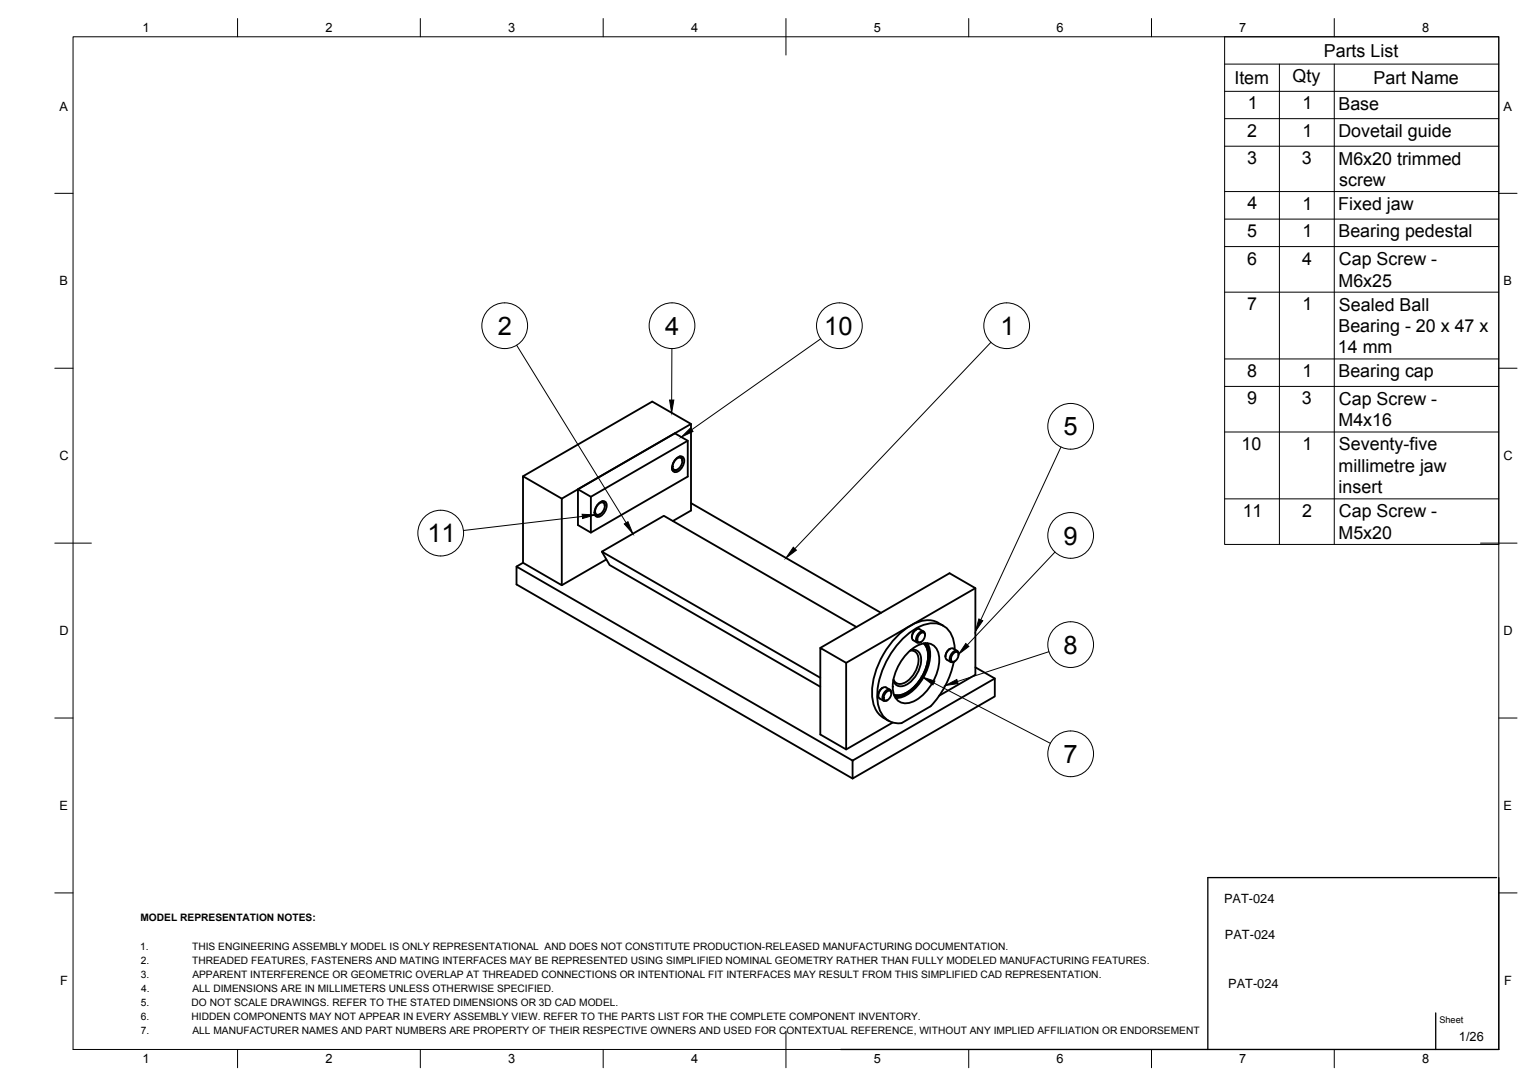
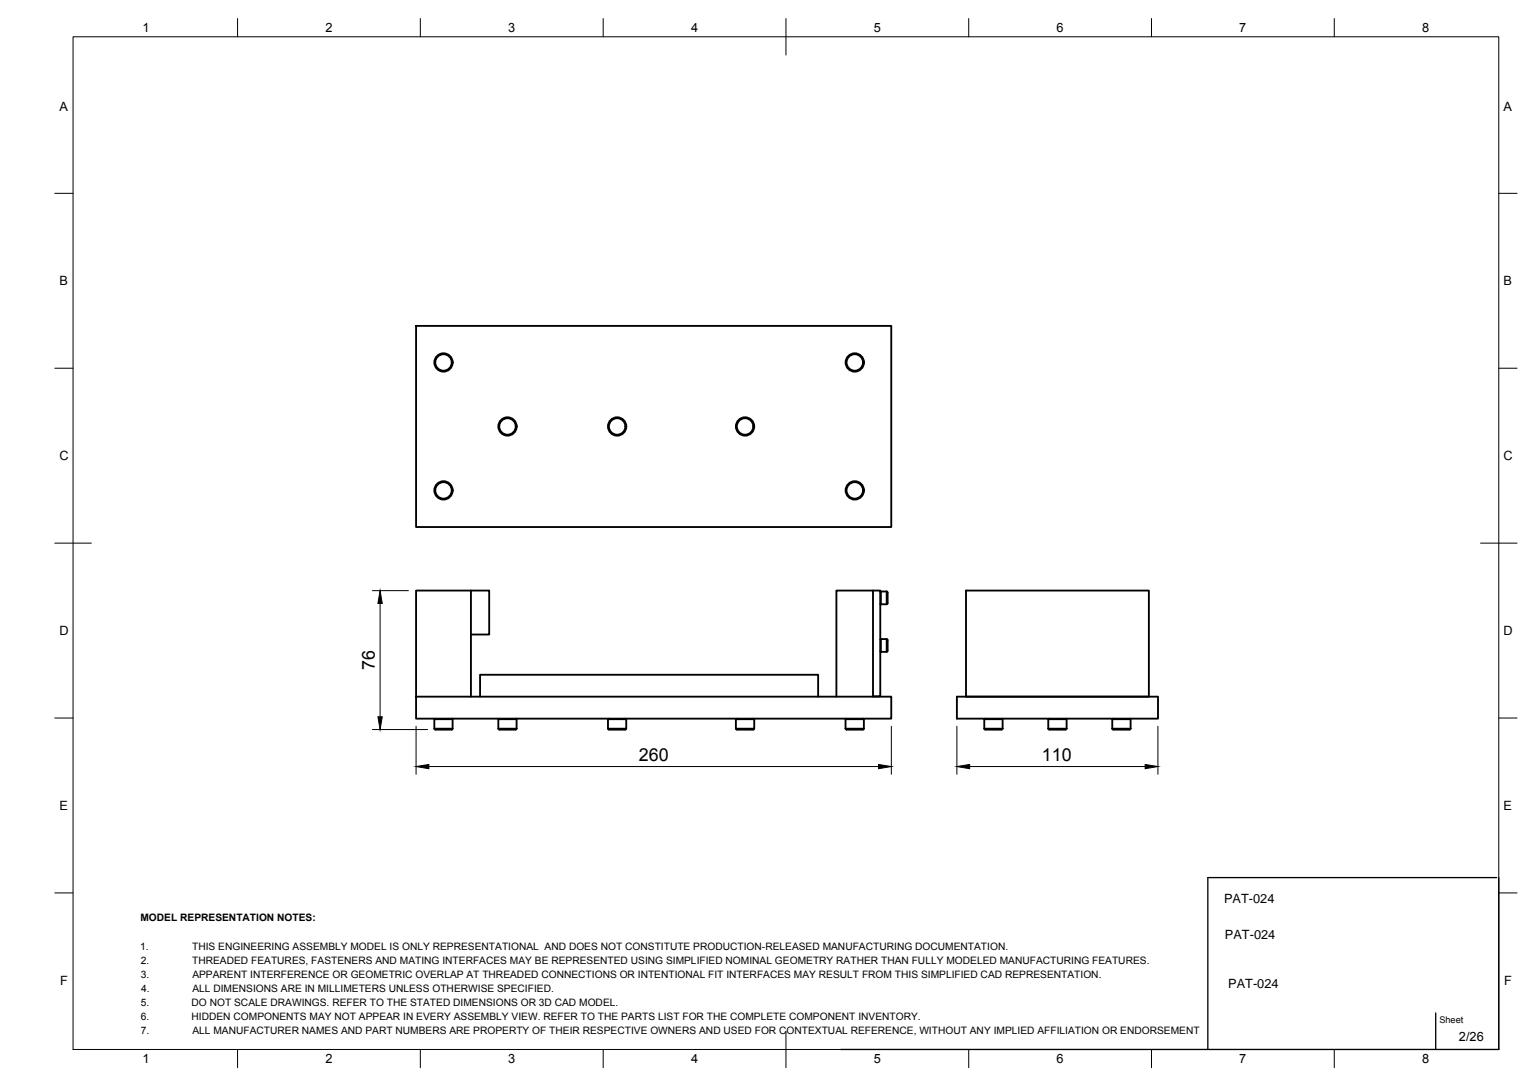
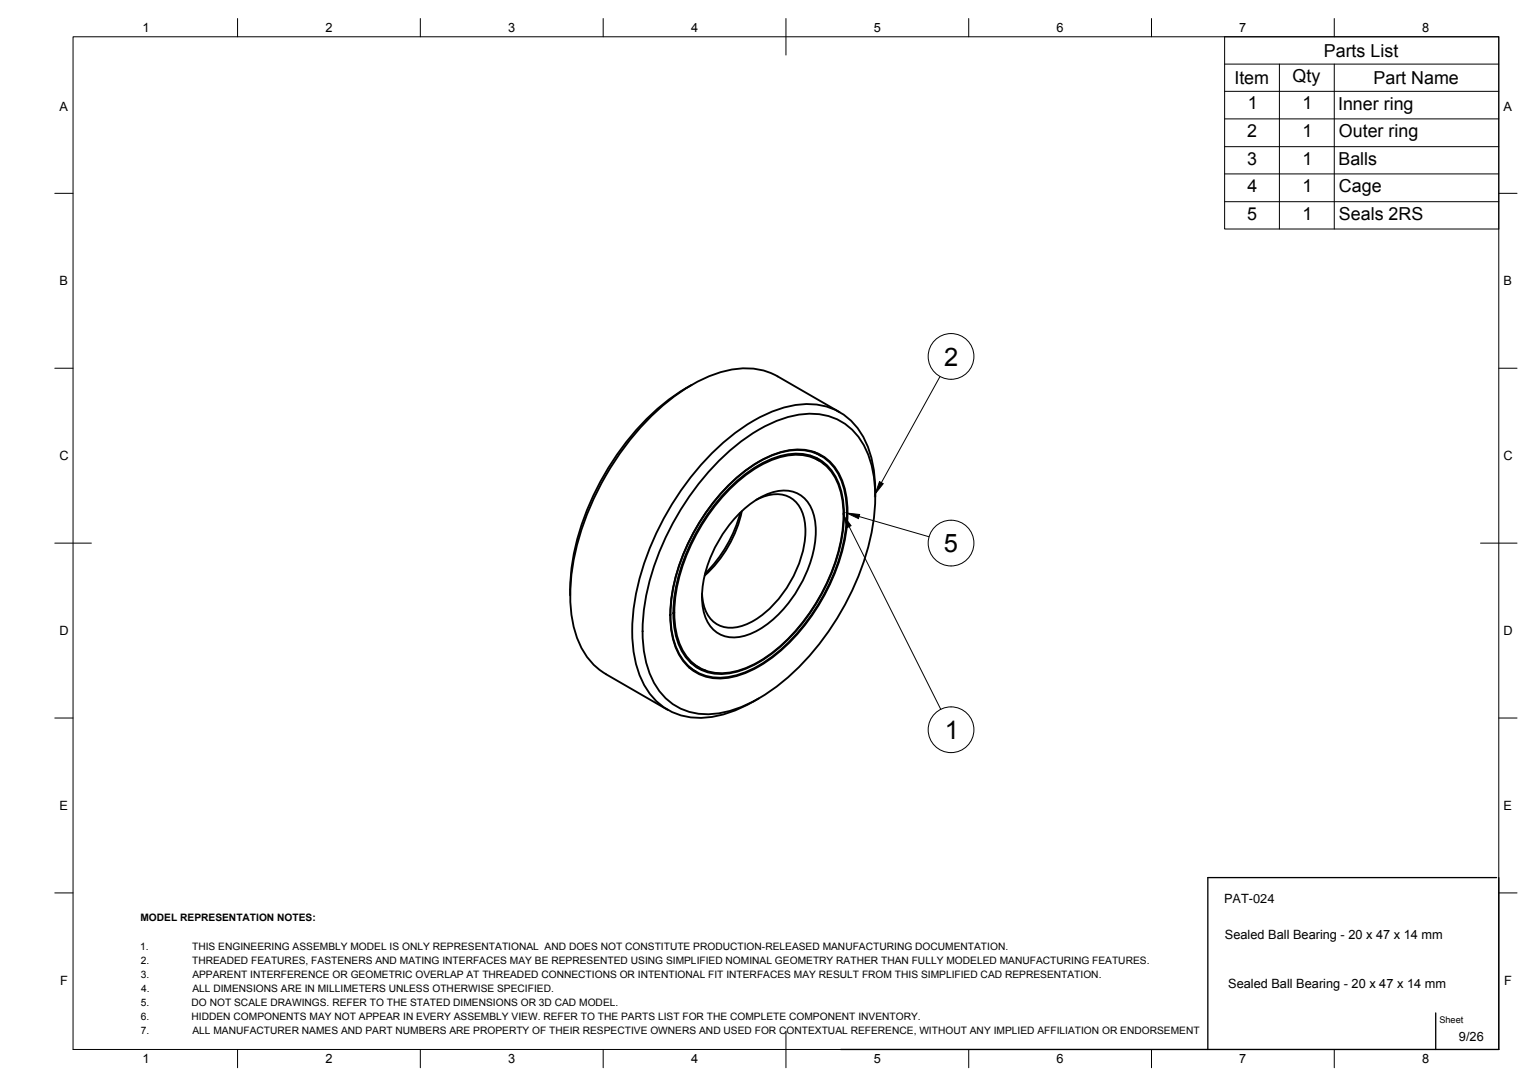
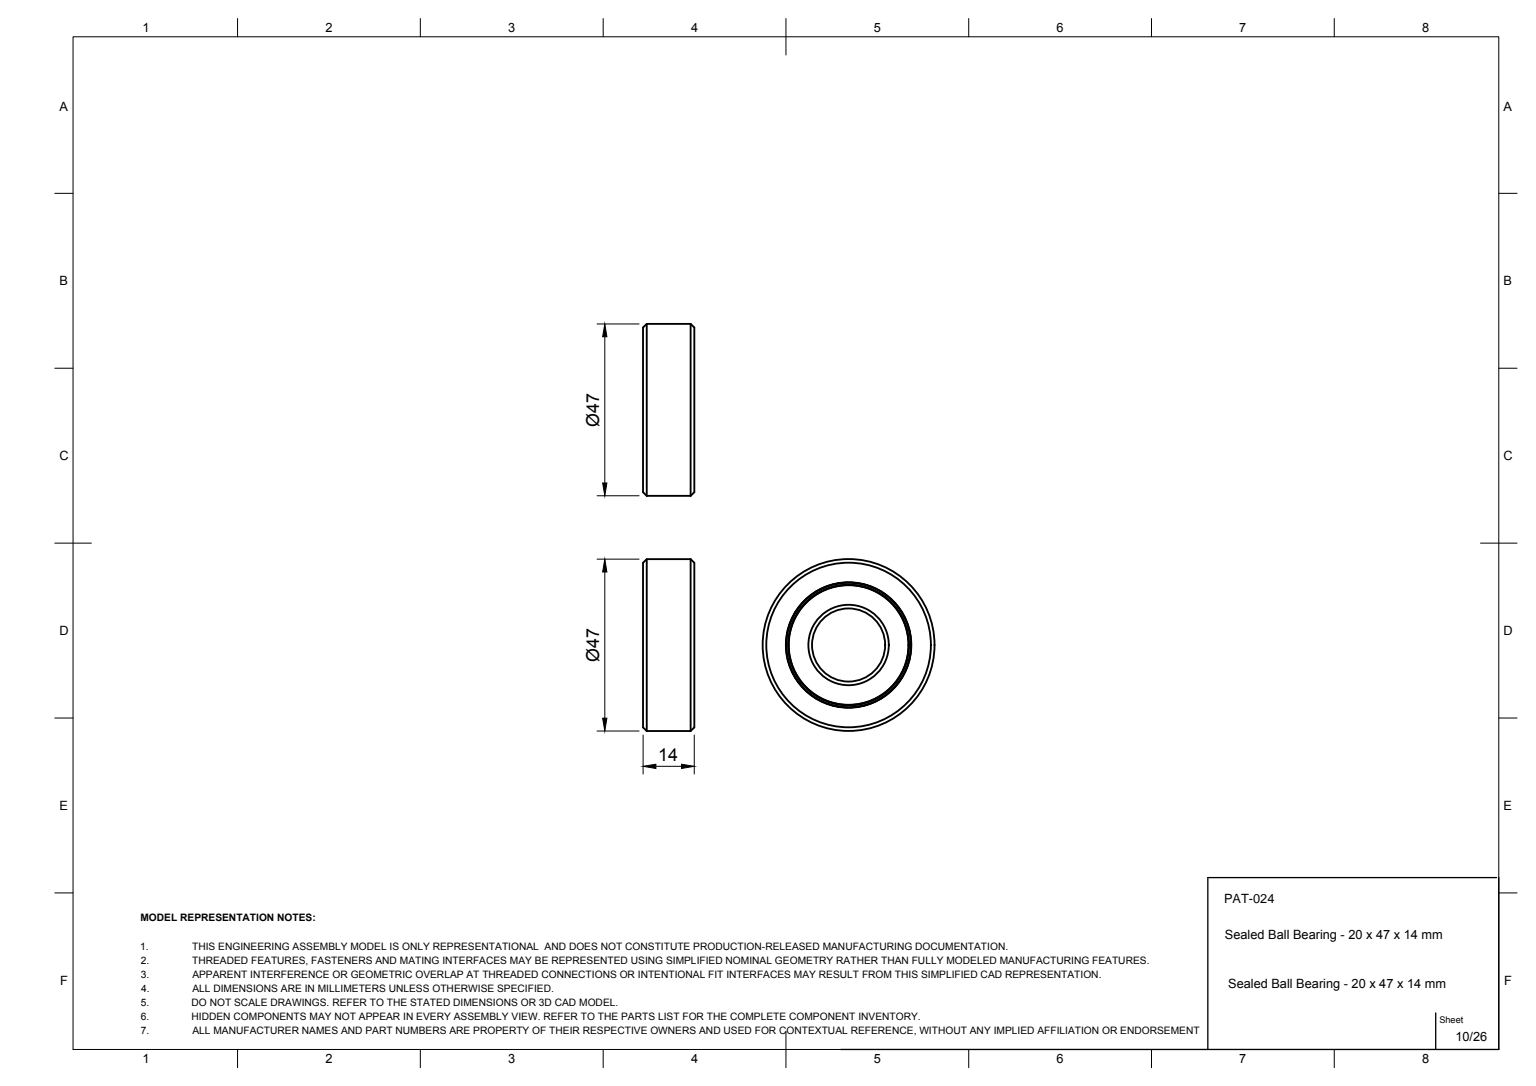
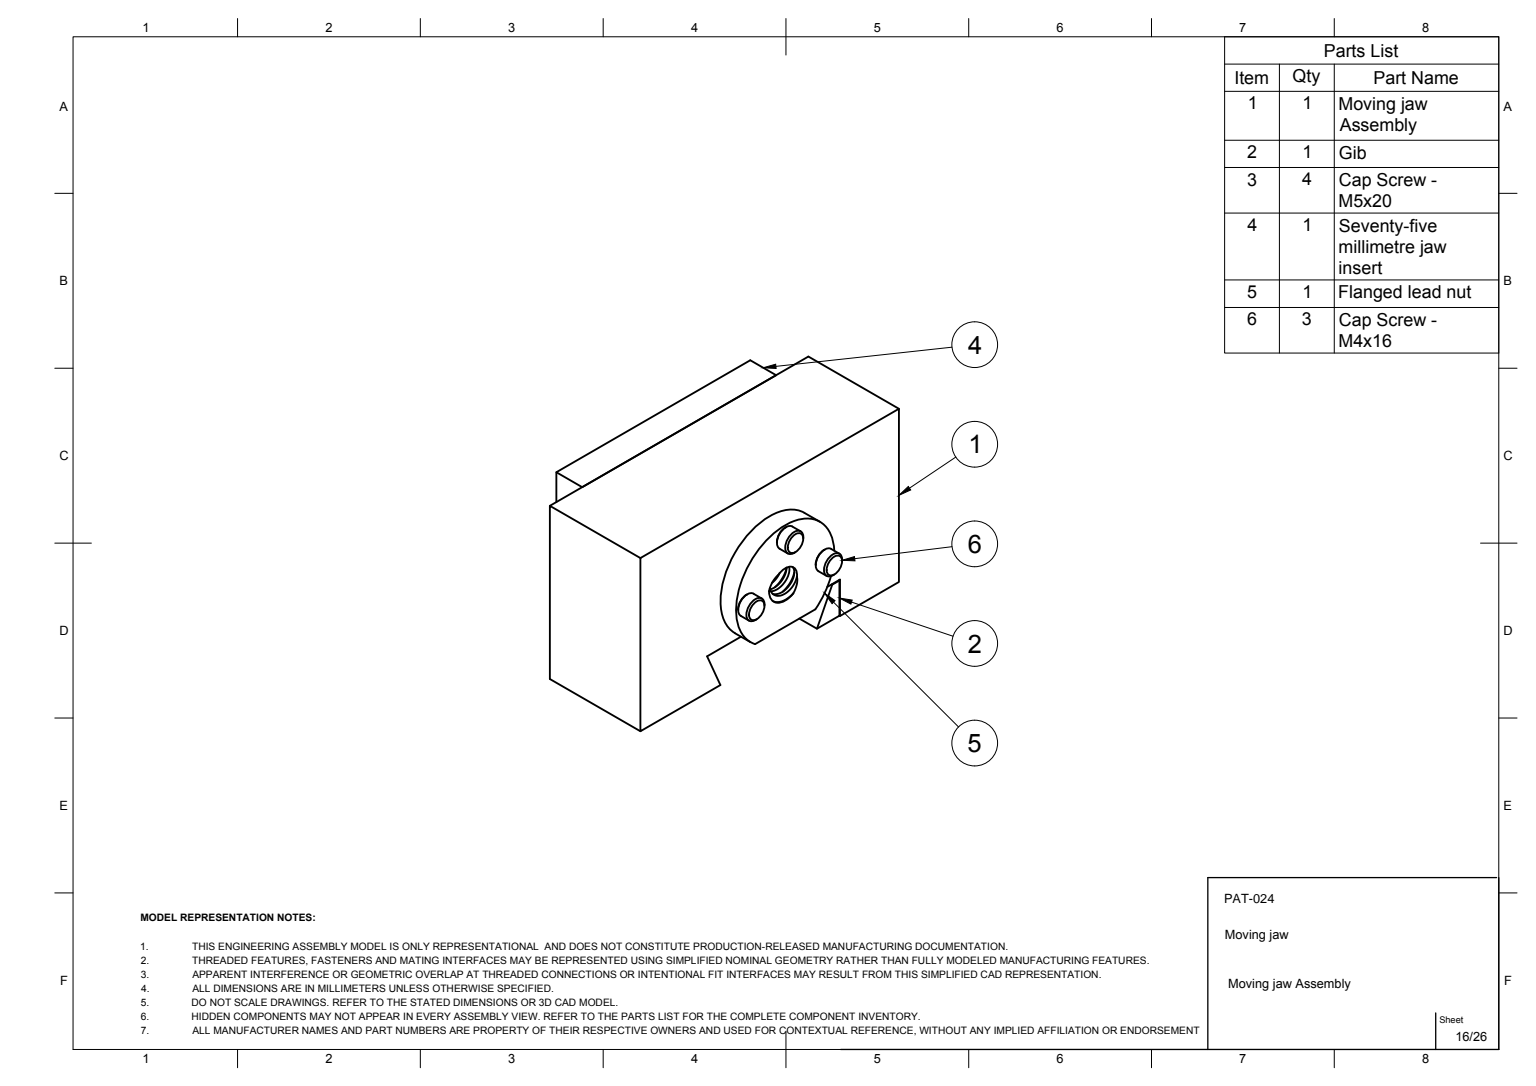
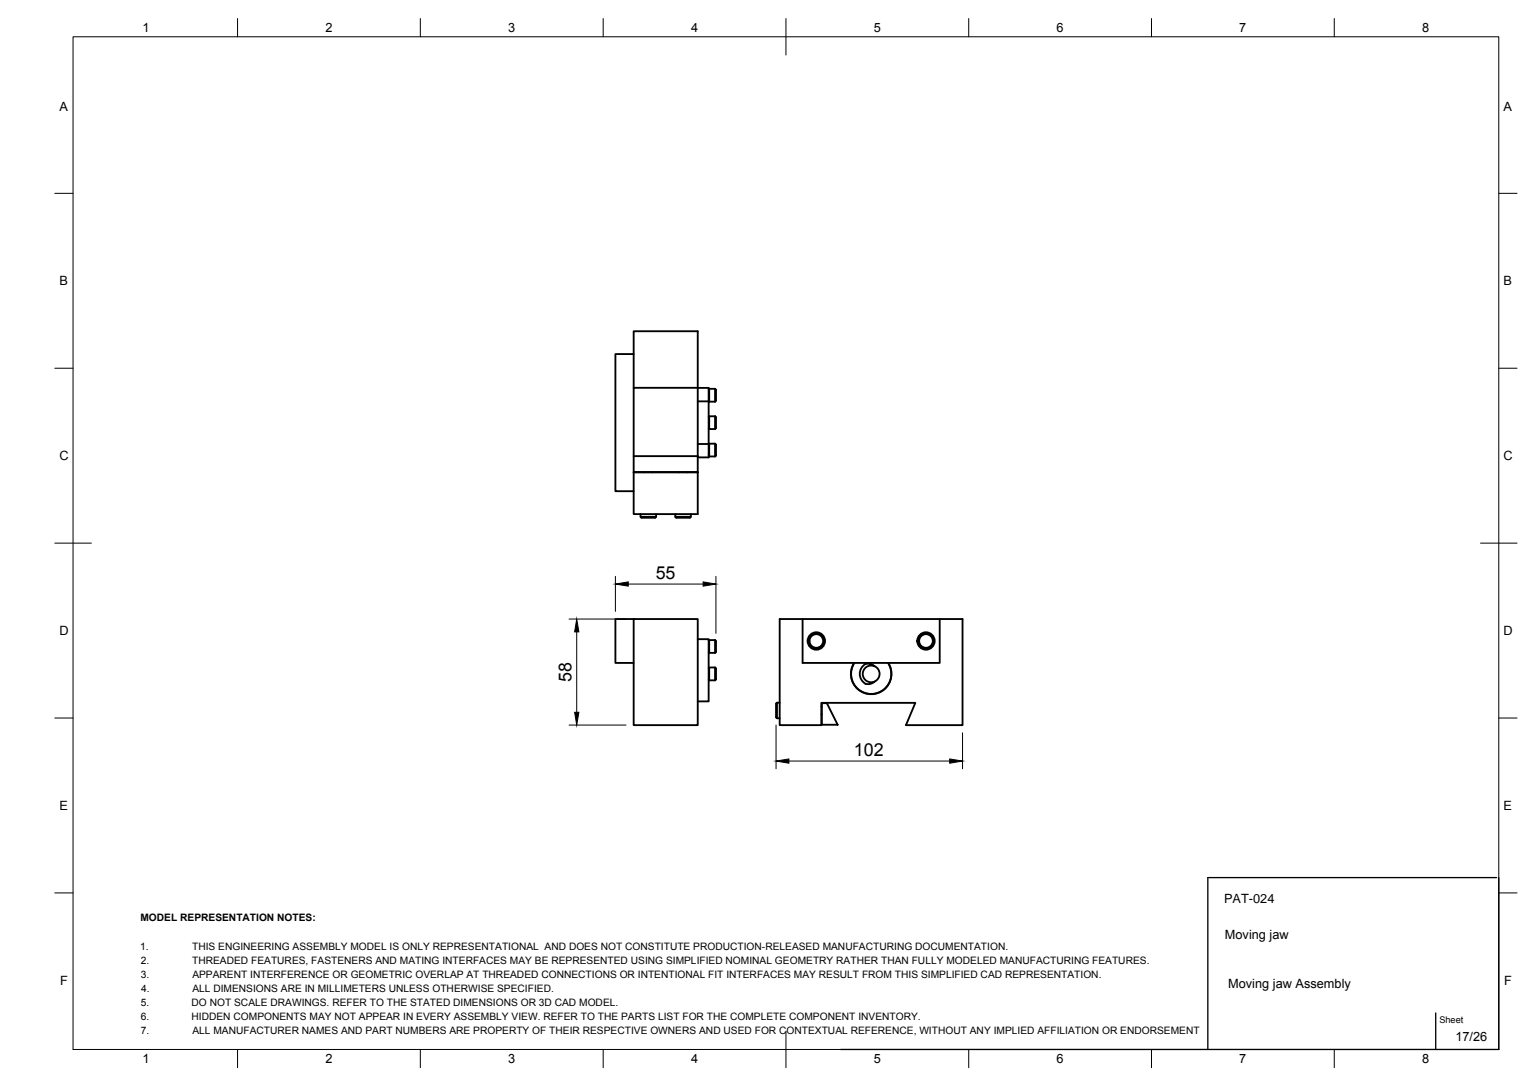
ISO-10303-21;
HEADER;
/* Generated by software containing ST-Developer
 * from STEP Tools, Inc. (www.steptools.com) 
 */

FILE_DESCRIPTION(
/* description */ ('Compact handwheel screw vise'),
/* implementation_level */ '2;1');

FILE_NAME(
/* name */ 'PAT-024',
/* time_stamp */ '2026-10-29T16:08:22-07:00',
/* author */ (''),
/* organization */ (''),
/* preprocessor_version */ 'ST-DEVELOPER v20.2',
/* originating_system */ 'Autodesk Translation Framework v15.17.0.0',
/* authorisation */ '');

FILE_SCHEMA (('AUTOMOTIVE_DESIGN { 1 0 10303 214 3 1 1 }'));
ENDSEC;

DATA;
#10=MECHANICAL_DESIGN_GEOMETRIC_PRESENTATION_REPRESENTATION('',(#644,#645,
#646,#647,#648,#649,#650,#651,#652,#653,#654,#655,#656,#657,#658,#659,#660,
#661,#662,#663,#664,#665,#666,#667,#668,#669,#670,#671,#672,#673,#674,#675,
#676,#677,#678,#679),#25074);
#11=B_SPLINE_SURFACE_WITH_KNOTS('',3,3,((#13564,#13565,#13566,#13567,#13568,
#13569,#13570,#13571,#13572,#13573,#13574,#13575,#13576,#13577,#13578,#13579,
#13580,#13581,#13582,#13583,#13584,#13585,#13586,#13587,#13588,#13589,#13590,
#13591,#13592,#13593,#13594,#13595,#13596,#13597,#13598,#13599,#13600,#13601,
#13602,#13603,#13604,#13605,#13606,#13607,#13608,#13609,#13610,#13611,#13612,
#13613,#13614,#13615,#13616,#13617,#13618,#13619,#13620,#13621,#13622,#13623,
#13624,#13625,#13626,#13627,#13628,#13629,#13630,#13631,#13632,#13633,#13634,
#13635,#13636,#13637,#13638,#13639,#13640,#13641,#13642,#13643,#13644,#13645,
#13646,#13647,#13648,#13649,#13650,#13651,#13652,#13653,#13654,#13655,#13656,
#13657,#13658,#13659,#13660,#13661,#13662,#13663,#13664,#13665,#13666,#13667,
#13668,#13669,#13670,#13671,#13672,#13673,#13674,#13675,#13676,#13677,#13678),
(#13679,#13680,#13681,#13682,#13683,#13684,#13685,#13686,#13687,#13688,
#13689,#13690,#13691,#13692,#13693,#13694,#13695,#13696,#13697,#13698,#13699,
#13700,#13701,#13702,#13703,#13704,#13705,#13706,#13707,#13708,#13709,#13710,
#13711,#13712,#13713,#13714,#13715,#13716,#13717,#13718,#13719,#13720,#13721,
#13722,#13723,#13724,#13725,#13726,#13727,#13728,#13729,#13730,#13731,#13732,
#13733,#13734,#13735,#13736,#13737,#13738,#13739,#13740,#13741,#13742,#13743,
#13744,#13745,#13746,#13747,#13748,#13749,#13750,#13751,#13752,#13753,#13754,
#13755,#13756,#13757,#13758,#13759,#13760,#13761,#13762,#13763,#13764,#13765,
#13766,#13767,#13768,#13769,#13770,#13771,#13772,#13773,#13774,#13775,#13776,
#13777,#13778,#13779,#13780,#13781,#13782,#13783,#13784,#13785,#13786,#13787,
#13788,#13789,#13790,#13791,#13792,#13793),(#13794,#13795,#13796,#13797,
#13798,#13799,#13800,#13801,#13802,#13803,#13804,#13805,#13806,#13807,#13808,
#13809,#13810,#13811,#13812,#13813,#13814,#13815,#13816,#13817,#13818,#13819,
#13820,#13821,#13822,#13823,#13824,#13825,#13826,#13827,#13828,#13829,#13830,
#13831,#13832,#13833,#13834,#13835,#13836,#13837,#13838,#13839,#13840,#13841,
#13842,#13843,#13844,#13845,#13846,#13847,#13848,#13849,#13850,#13851,#13852,
#13853,#13854,#13855,#13856,#13857,#13858,#13859,#13860,#13861,#13862,#13863,
#13864,#13865,#13866,#13867,#13868,#13869,#13870,#13871,#13872,#13873,#13874,
#13875,#13876,#13877,#13878,#13879,#13880,#13881,#13882,#13883,#13884,#13885,
#13886,#13887,#13888,#13889,#13890,#13891,#13892,#13893,#13894,#13895,#13896,
#13897,#13898,#13899,#13900,#13901,#13902,#13903,#13904,#13905,#13906,#13907,
#13908),(#13909,#13910,#13911,#13912,#13913,#13914,#13915,#13916,#13917,
#13918,#13919,#13920,#13921,#13922,#13923,#13924,#13925,#13926,#13927,#13928,
#13929,#13930,#13931,#13932,#13933,#13934,#13935,#13936,#13937,#13938,#13939,
#13940,#13941,#13942,#13943,#13944,#13945,#13946,#13947,#13948,#13949,#13950,
#13951,#13952,#13953,#13954,#13955,#13956,#13957,#13958,#13959,#13960,#13961,
#13962,#13963,#13964,#13965,#13966,#13967,#13968,#13969,#13970,#13971,#13972,
#13973,#13974,#13975,#13976,#13977,#13978,#13979,#13980,#13981,#13982,#13983,
#13984,#13985,#13986,#13987,#13988,#13989,#13990,#13991,#13992,#13993,#13994,
#13995,#13996,#13997,#13998,#13999,#14000,#14001,#14002,#14003,#14004,#14005,
#14006,#14007,#14008,#14009,#14010,#14011,#14012,#14013,#14014,#14015,#14016,
#14017,#14018,#14019,#14020,#14021,#14022,#14023)),.UNSPECIFIED.,.F.,.F.,
 .F.,(4,4),(4,1,1,1,1,1,1,1,1,1,1,1,1,1,1,1,1,1,1,1,1,1,1,1,1,1,1,1,1,1,
1,1,1,1,1,1,1,1,1,1,1,1,1,1,1,1,1,1,1,1,1,1,1,1,1,1,1,1,1,1,1,1,1,1,1,1,
1,1,1,1,1,1,1,1,1,1,1,1,1,1,1,1,1,1,1,1,1,1,1,1,1,1,1,1,1,1,1,1,1,1,1,1,
1,1,1,1,1,1,1,1,1,1,4),(0.,0.173020531651036),(12.1475814751569,12.6421543672732,
13.1367272593894,13.6313001515056,14.1258730436219,14.6204459357381,15.1150188278544,
15.6095917199706,16.1041646120869,16.5987375042031,17.0933103963194,17.5878832884356,
18.0824561805519,18.5770290726681,19.0716019647843,19.5661748569006,20.0607477490168,
20.5553206411331,21.0498935332493,21.5444664253656,22.0390393174818,22.5336122095981,
23.0281851017143,23.5227579938306,24.0173308859468,24.511903778063,25.0064766701793,
25.5010495622955,25.9956224544118,26.490195346528,26.9847682386443,27.4793411307605,
27.9739140228768,28.468486914993,28.9630598071093,29.4576326992255,29.9522055913417,
30.446778483458,30.9413513755742,31.4359242676905,31.9304971598067,32.425070051923,
32.9196429440392,33.4142158361555,33.9087887282717,34.403361620388,34.8979345125042,
35.3925074046204,35.8870802967367,36.3816531888529,36.8762260809692,37.3707989730854,
37.8653718652017,38.3599447573179,38.8545176494342,39.3490905415504,39.8436634336667,
40.3382363257829,40.8328092178991,41.3273821100154,41.8219550021316,42.3165278942479,
42.8111007863641,43.3056736784804,43.8002465705966,44.2948194627129,44.7893923548291,
45.2839652469454,45.7785381390616,46.2731110311778,46.7676839232941,47.2622568154103,
47.7568297075266,48.2514025996428,48.7459754917591,49.2405483838753,49.7351212759916,
50.2296941681078,50.7242670602241,51.2188399523403,51.7134128444565,52.2079857365728,
52.702558628689,53.1971315208053,53.6917044129215,54.1862773050378,54.680850197154,
55.1754230892703,55.6699959813865,56.1645688735028,56.659141765619,57.1537146577353,
57.6482875498515,58.1428604419677,58.637433334084,59.1320062262002,59.6265791183165,
60.1211520104327,60.615724902549,61.1102977946652,61.6048706867815,62.0994435788977,
62.5940164710139,63.0885893631302,63.5831622552464,64.0777351473627,64.5723080394789,
65.0668809315952,65.5614538237114,66.0560267158277,66.5505996079439,67.0451725000601,
67.5397453921764),.UNSPECIFIED.);
#12=B_SPLINE_SURFACE_WITH_KNOTS('',3,3,((#14123,#14124,#14125,#14126,#14127,
#14128,#14129,#14130,#14131,#14132,#14133,#14134,#14135,#14136,#14137,#14138,
#14139,#14140,#14141,#14142,#14143,#14144,#14145,#14146,#14147,#14148,#14149,
#14150,#14151,#14152,#14153,#14154,#14155,#14156,#14157,#14158,#14159,#14160,
#14161,#14162,#14163,#14164,#14165,#14166,#14167,#14168,#14169,#14170,#14171,
#14172,#14173,#14174,#14175,#14176,#14177,#14178,#14179,#14180,#14181,#14182,
#14183,#14184,#14185,#14186,#14187,#14188,#14189,#14190,#14191,#14192,#14193,
#14194,#14195,#14196,#14197,#14198,#14199,#14200,#14201,#14202,#14203,#14204,
#14205,#14206,#14207,#14208,#14209,#14210,#14211,#14212,#14213,#14214,#14215,
#14216,#14217,#14218,#14219,#14220,#14221,#14222,#14223,#14224,#14225,#14226,
#14227,#14228,#14229,#14230,#14231,#14232,#14233,#14234,#14235,#14236,#14237),
(#14238,#14239,#14240,#14241,#14242,#14243,#14244,#14245,#14246,#14247,
#14248,#14249,#14250,#14251,#14252,#14253,#14254,#14255,#14256,#14257,#14258,
#14259,#14260,#14261,#14262,#14263,#14264,#14265,#14266,#14267,#14268,#14269,
#14270,#14271,#14272,#14273,#14274,#14275,#14276,#14277,#14278,#14279,#14280,
#14281,#14282,#14283,#14284,#14285,#14286,#14287,#14288,#14289,#14290,#14291,
#14292,#14293,#14294,#14295,#14296,#14297,#14298,#14299,#14300,#14301,#14302,
#14303,#14304,#14305,#14306,#14307,#14308,#14309,#14310,#14311,#14312,#14313,
#14314,#14315,#14316,#14317,#14318,#14319,#14320,#14321,#14322,#14323,#14324,
#14325,#14326,#14327,#14328,#14329,#14330,#14331,#14332,#14333,#14334,#14335,
#14336,#14337,#14338,#14339,#14340,#14341,#14342,#14343,#14344,#14345,#14346,
#14347,#14348,#14349,#14350,#14351,#14352),(#14353,#14354,#14355,#14356,
#14357,#14358,#14359,#14360,#14361,#14362,#14363,#14364,#14365,#14366,#14367,
#14368,#14369,#14370,#14371,#14372,#14373,#14374,#14375,#14376,#14377,#14378,
#14379,#14380,#14381,#14382,#14383,#14384,#14385,#14386,#14387,#14388,#14389,
#14390,#14391,#14392,#14393,#14394,#14395,#14396,#14397,#14398,#14399,#14400,
#14401,#14402,#14403,#14404,#14405,#14406,#14407,#14408,#14409,#14410,#14411,
#14412,#14413,#14414,#14415,#14416,#14417,#14418,#14419,#14420,#14421,#14422,
#14423,#14424,#14425,#14426,#14427,#14428,#14429,#14430,#14431,#14432,#14433,
#14434,#14435,#14436,#14437,#14438,#14439,#14440,#14441,#14442,#14443,#14444,
#14445,#14446,#14447,#14448,#14449,#14450,#14451,#14452,#14453,#14454,#14455,
#14456,#14457,#14458,#14459,#14460,#14461,#14462,#14463,#14464,#14465,#14466,
#14467),(#14468,#14469,#14470,#14471,#14472,#14473,#14474,#14475,#14476,
#14477,#14478,#14479,#14480,#14481,#14482,#14483,#14484,#14485,#14486,#14487,
#14488,#14489,#14490,#14491,#14492,#14493,#14494,#14495,#14496,#14497,#14498,
#14499,#14500,#14501,#14502,#14503,#14504,#14505,#14506,#14507,#14508,#14509,
#14510,#14511,#14512,#14513,#14514,#14515,#14516,#14517,#14518,#14519,#14520,
#14521,#14522,#14523,#14524,#14525,#14526,#14527,#14528,#14529,#14530,#14531,
#14532,#14533,#14534,#14535,#14536,#14537,#14538,#14539,#14540,#14541,#14542,
#14543,#14544,#14545,#14546,#14547,#14548,#14549,#14550,#14551,#14552,#14553,
#14554,#14555,#14556,#14557,#14558,#14559,#14560,#14561,#14562,#14563,#14564,
#14565,#14566,#14567,#14568,#14569,#14570,#14571,#14572,#14573,#14574,#14575,
#14576,#14577,#14578,#14579,#14580,#14581,#14582)),.UNSPECIFIED.,.F.,.F.,
 .F.,(4,4),(4,1,1,1,1,1,1,1,1,1,1,1,1,1,1,1,1,1,1,1,1,1,1,1,1,1,1,1,1,1,
1,1,1,1,1,1,1,1,1,1,1,1,1,1,1,1,1,1,1,1,1,1,1,1,1,1,1,1,1,1,1,1,1,1,1,1,
1,1,1,1,1,1,1,1,1,1,1,1,1,1,1,1,1,1,1,1,1,1,1,1,1,1,1,1,1,1,1,1,1,1,1,1,
1,1,1,1,1,1,1,1,1,1,4),(0.,0.173020531651036),(15.1888611523549,15.6834340444711,
16.1780069365874,16.6725798287036,17.1671527208199,17.6617256129361,18.1562985050523,
18.6508713971686,19.1454442892848,19.6400171814011,20.1345900735173,20.6291629656336,
21.1237358577498,21.6183087498661,22.1128816419823,22.6074545340986,23.1020274262148,
23.596600318331,24.0911732104473,24.5857461025635,25.0803189946798,25.574891886796,
26.0694647789123,26.5640376710285,27.0586105631448,27.553183455261,28.0477563473773,
28.5423292394935,29.0369021316097,29.531475023726,30.0260479158422,30.5206208079585,
31.0151937000747,31.509766592191,32.0043394843072,32.4989123764235,32.9934852685397,
33.488058160656,33.9826310527722,34.4772039448884,34.9717768370047,35.4663497291209,
35.9609226212372,36.4554955133534,36.9500684054697,37.4446412975859,37.9392141897022,
38.4337870818184,38.9283599739347,39.4229328660509,39.9175057581671,40.4120786502834,
40.9066515423996,41.4012244345159,41.8957973266321,42.3903702187484,42.8849431108646,
43.3795160029809,43.8740888950971,44.3686617872134,44.8632346793296,45.3578075714458,
45.8523804635621,46.3469533556783,46.8415262477946,47.3360991399108,47.8306720320271,
48.3252449241433,48.8198178162596,49.3143907083758,49.8089636004921,50.3035364926083,
50.7981093847245,51.2926822768408,51.787255168957,52.2818280610733,52.7764009531895,
53.2709738453058,53.765546737422,54.2601196295383,54.7546925216545,55.2492654137708,
55.743838305887,56.2384111980032,56.7329840901195,57.2275569822357,57.722129874352,
58.2167027664682,58.7112756585845,59.2058485507007,59.700421442817,60.1949943349332,
60.6895672270495,61.1841401191657,61.6787130112819,62.1732859033982,62.6678587955144,
63.1624316876307,63.6570045797469,64.1515774718632,64.6461503639794,65.1407232560957,
65.6352961482119,66.1298690403281,66.6244419324444,67.1190148245607,67.6135877166769,
68.1081606087931,68.6027335009094,69.0973063930256,69.5918792851419,70.0864521772581,
70.5810250693744),.UNSPECIFIED.);
#13=B_SPLINE_SURFACE_WITH_KNOTS('',3,3,((#20271,#20272,#20273,#20274,#20275,
#20276,#20277,#20278,#20279,#20280,#20281,#20282,#20283,#20284,#20285,#20286,
#20287,#20288,#20289,#20290,#20291,#20292,#20293,#20294,#20295,#20296,#20297,
#20298,#20299,#20300,#20301,#20302,#20303,#20304,#20305,#20306,#20307,#20308,
#20309,#20310,#20311,#20312,#20313,#20314,#20315,#20316,#20317,#20318,#20319,
#20320,#20321,#20322,#20323,#20324,#20325,#20326,#20327,#20328,#20329,#20330,
#20331,#20332,#20333,#20334,#20335,#20336,#20337,#20338,#20339,#20340,#20341,
#20342,#20343,#20344,#20345,#20346,#20347,#20348,#20349,#20350,#20351,#20352,
#20353,#20354,#20355,#20356,#20357,#20358,#20359,#20360,#20361,#20362,#20363,
#20364,#20365,#20366,#20367,#20368,#20369,#20370,#20371,#20372,#20373,#20374,
#20375,#20376,#20377,#20378,#20379,#20380,#20381,#20382,#20383,#20384,#20385,
#20386,#20387,#20388,#20389,#20390,#20391,#20392,#20393,#20394,#20395,#20396,
#20397,#20398,#20399,#20400,#20401,#20402,#20403,#20404,#20405,#20406,#20407,
#20408,#20409,#20410,#20411,#20412,#20413,#20414,#20415,#20416,#20417,#20418,
#20419,#20420,#20421,#20422,#20423,#20424,#20425,#20426,#20427,#20428,#20429,
#20430,#20431,#20432,#20433,#20434,#20435,#20436,#20437,#20438,#20439,#20440,
#20441,#20442,#20443,#20444,#20445,#20446,#20447,#20448,#20449,#20450,#20451,
#20452,#20453,#20454,#20455,#20456,#20457,#20458,#20459,#20460,#20461,#20462,
#20463,#20464,#20465,#20466,#20467,#20468,#20469,#20470,#20471,#20472,#20473,
#20474,#20475,#20476,#20477,#20478,#20479,#20480,#20481,#20482,#20483,#20484,
#20485,#20486,#20487,#20488,#20489,#20490,#20491,#20492,#20493,#20494,#20495,
#20496,#20497,#20498,#20499,#20500,#20501,#20502,#20503,#20504,#20505,#20506,
#20507,#20508,#20509,#20510,#20511,#20512,#20513,#20514,#20515,#20516,#20517,
#20518,#20519,#20520,#20521,#20522,#20523,#20524,#20525,#20526,#20527,#20528,
#20529,#20530,#20531,#20532,#20533,#20534,#20535,#20536,#20537,#20538,#20539,
#20540,#20541,#20542,#20543,#20544,#20545,#20546,#20547,#20548,#20549,#20550,
#20551,#20552,#20553,#20554,#20555,#20556,#20557,#20558,#20559,#20560,#20561,
#20562,#20563,#20564,#20565,#20566,#20567,#20568,#20569,#20570,#20571,#20572,
#20573,#20574,#20575,#20576,#20577,#20578,#20579,#20580,#20581,#20582,#20583,
#20584,#20585,#20586,#20587,#20588,#20589,#20590,#20591,#20592,#20593,#20594,
#20595,#20596,#20597,#20598,#20599,#20600,#20601,#20602,#20603,#20604,#20605,
#20606,#20607,#20608,#20609,#20610,#20611,#20612,#20613,#20614,#20615,#20616,
#20617,#20618,#20619,#20620,#20621,#20622,#20623,#20624,#20625,#20626,#20627,
#20628,#20629,#20630,#20631,#20632,#20633,#20634,#20635,#20636,#20637,#20638,
#20639,#20640,#20641,#20642,#20643,#20644,#20645,#20646,#20647,#20648,#20649,
#20650,#20651,#20652,#20653,#20654,#20655,#20656,#20657,#20658,#20659,#20660,
#20661,#20662,#20663,#20664,#20665,#20666,#20667,#20668,#20669,#20670,#20671,
#20672,#20673,#20674,#20675,#20676,#20677,#20678,#20679,#20680,#20681,#20682,
#20683,#20684,#20685,#20686,#20687,#20688,#20689,#20690,#20691,#20692,#20693,
#20694,#20695,#20696,#20697,#20698,#20699,#20700,#20701,#20702,#20703,#20704,
#20705,#20706,#20707,#20708,#20709,#20710,#20711,#20712,#20713,#20714,#20715,
#20716,#20717,#20718,#20719,#20720,#20721,#20722,#20723,#20724,#20725,#20726,
#20727,#20728,#20729,#20730,#20731,#20732,#20733,#20734,#20735,#20736,#20737,
#20738,#20739,#20740,#20741,#20742,#20743,#20744,#20745,#20746,#20747,#20748,
#20749,#20750,#20751,#20752,#20753,#20754,#20755,#20756,#20757,#20758,#20759,
#20760,#20761,#20762,#20763,#20764,#20765,#20766,#20767,#20768),(#20769,
#20770,#20771,#20772,#20773,#20774,#20775,#20776,#20777,#20778,#20779,#20780,
#20781,#20782,#20783,#20784,#20785,#20786,#20787,#20788,#20789,#20790,#20791,
#20792,#20793,#20794,#20795,#20796,#20797,#20798,#20799,#20800,#20801,#20802,
#20803,#20804,#20805,#20806,#20807,#20808,#20809,#20810,#20811,#20812,#20813,
#20814,#20815,#20816,#20817,#20818,#20819,#20820,#20821,#20822,#20823,#20824,
#20825,#20826,#20827,#20828,#20829,#20830,#20831,#20832,#20833,#20834,#20835,
#20836,#20837,#20838,#20839,#20840,#20841,#20842,#20843,#20844,#20845,#20846,
#20847,#20848,#20849,#20850,#20851,#20852,#20853,#20854,#20855,#20856,#20857,
#20858,#20859,#20860,#20861,#20862,#20863,#20864,#20865,#20866,#20867,#20868,
#20869,#20870,#20871,#20872,#20873,#20874,#20875,#20876,#20877,#20878,#20879,
#20880,#20881,#20882,#20883,#20884,#20885,#20886,#20887,#20888,#20889,#20890,
#20891,#20892,#20893,#20894,#20895,#20896,#20897,#20898,#20899,#20900,#20901,
#20902,#20903,#20904,#20905,#20906,#20907,#20908,#20909,#20910,#20911,#20912,
#20913,#20914,#20915,#20916,#20917,#20918,#20919,#20920,#20921,#20922,#20923,
#20924,#20925,#20926,#20927,#20928,#20929,#20930,#20931,#20932,#20933,#20934,
#20935,#20936,#20937,#20938,#20939,#20940,#20941,#20942,#20943,#20944,#20945,
#20946,#20947,#20948,#20949,#20950,#20951,#20952,#20953,#20954,#20955,#20956,
#20957,#20958,#20959,#20960,#20961,#20962,#20963,#20964,#20965,#20966,#20967,
#20968,#20969,#20970,#20971,#20972,#20973,#20974,#20975,#20976,#20977,#20978,
#20979,#20980,#20981,#20982,#20983,#20984,#20985,#20986,#20987,#20988,#20989,
#20990,#20991,#20992,#20993,#20994,#20995,#20996,#20997,#20998,#20999,#21000,
#21001,#21002,#21003,#21004,#21005,#21006,#21007,#21008,#21009,#21010,#21011,
#21012,#21013,#21014,#21015,#21016,#21017,#21018,#21019,#21020,#21021,#21022,
#21023,#21024,#21025,#21026,#21027,#21028,#21029,#21030,#21031,#21032,#21033,
#21034,#21035,#21036,#21037,#21038,#21039,#21040,#21041,#21042,#21043,#21044,
#21045,#21046,#21047,#21048,#21049,#21050,#21051,#21052,#21053,#21054,#21055,
#21056,#21057,#21058,#21059,#21060,#21061,#21062,#21063,#21064,#21065,#21066,
#21067,#21068,#21069,#21070,#21071,#21072,#21073,#21074,#21075,#21076,#21077,
#21078,#21079,#21080,#21081,#21082,#21083,#21084,#21085,#21086,#21087,#21088,
#21089,#21090,#21091,#21092,#21093,#21094,#21095,#21096,#21097,#21098,#21099,
#21100,#21101,#21102,#21103,#21104,#21105,#21106,#21107,#21108,#21109,#21110,
#21111,#21112,#21113,#21114,#21115,#21116,#21117,#21118,#21119,#21120,#21121,
#21122,#21123,#21124,#21125,#21126,#21127,#21128,#21129,#21130,#21131,#21132,
#21133,#21134,#21135,#21136,#21137,#21138,#21139,#21140,#21141,#21142,#21143,
#21144,#21145,#21146,#21147,#21148,#21149,#21150,#21151,#21152,#21153,#21154,
#21155,#21156,#21157,#21158,#21159,#21160,#21161,#21162,#21163,#21164,#21165,
#21166,#21167,#21168,#21169,#21170,#21171,#21172,#21173,#21174,#21175,#21176,
#21177,#21178,#21179,#21180,#21181,#21182,#21183,#21184,#21185,#21186,#21187,
#21188,#21189,#21190,#21191,#21192,#21193,#21194,#21195,#21196,#21197,#21198,
#21199,#21200,#21201,#21202,#21203,#21204,#21205,#21206,#21207,#21208,#21209,
#21210,#21211,#21212,#21213,#21214,#21215,#21216,#21217,#21218,#21219,#21220,
#21221,#21222,#21223,#21224,#21225,#21226,#21227,#21228,#21229,#21230,#21231,
#21232,#21233,#21234,#21235,#21236,#21237,#21238,#21239,#21240,#21241,#21242,
#21243,#21244,#21245,#21246,#21247,#21248,#21249,#21250,#21251,#21252,#21253,
#21254,#21255,#21256,#21257,#21258,#21259,#21260,#21261,#21262,#21263,#21264,
#21265,#21266),(#21267,#21268,#21269,#21270,#21271,#21272,#21273,#21274,
#21275,#21276,#21277,#21278,#21279,#21280,#21281,#21282,#21283,#21284,#21285,
#21286,#21287,#21288,#21289,#21290,#21291,#21292,#21293,#21294,#21295,#21296,
#21297,#21298,#21299,#21300,#21301,#21302,#21303,#21304,#21305,#21306,#21307,
#21308,#21309,#21310,#21311,#21312,#21313,#21314,#21315,#21316,#21317,#21318,
#21319,#21320,#21321,#21322,#21323,#21324,#21325,#21326,#21327,#21328,#21329,
#21330,#21331,#21332,#21333,#21334,#21335,#21336,#21337,#21338,#21339,#21340,
#21341,#21342,#21343,#21344,#21345,#21346,#21347,#21348,#21349,#21350,#21351,
#21352,#21353,#21354,#21355,#21356,#21357,#21358,#21359,#21360,#21361,#21362,
#21363,#21364,#21365,#21366,#21367,#21368,#21369,#21370,#21371,#21372,#21373,
#21374,#21375,#21376,#21377,#21378,#21379,#21380,#21381,#21382,#21383,#21384,
#21385,#21386,#21387,#21388,#21389,#21390,#21391,#21392,#21393,#21394,#21395,
#21396,#21397,#21398,#21399,#21400,#21401,#21402,#21403,#21404,#21405,#21406,
#21407,#21408,#21409,#21410,#21411,#21412,#21413,#21414,#21415,#21416,#21417,
#21418,#21419,#21420,#21421,#21422,#21423,#21424,#21425,#21426,#21427,#21428,
#21429,#21430,#21431,#21432,#21433,#21434,#21435,#21436,#21437,#21438,#21439,
#21440,#21441,#21442,#21443,#21444,#21445,#21446,#21447,#21448,#21449,#21450,
#21451,#21452,#21453,#21454,#21455,#21456,#21457,#21458,#21459,#21460,#21461,
#21462,#21463,#21464,#21465,#21466,#21467,#21468,#21469,#21470,#21471,#21472,
#21473,#21474,#21475,#21476,#21477,#21478,#21479,#21480,#21481,#21482,#21483,
#21484,#21485,#21486,#21487,#21488,#21489,#21490,#21491,#21492,#21493,#21494,
#21495,#21496,#21497,#21498,#21499,#21500,#21501,#21502,#21503,#21504,#21505,
#21506,#21507,#21508,#21509,#21510,#21511,#21512,#21513,#21514,#21515,#21516,
#21517,#21518,#21519,#21520,#21521,#21522,#21523,#21524,#21525,#21526,#21527,
#21528,#21529,#21530,#21531,#21532,#21533,#21534,#21535,#21536,#21537,#21538,
#21539,#21540,#21541,#21542,#21543,#21544,#21545,#21546,#21547,#21548,#21549,
#21550,#21551,#21552,#21553,#21554,#21555,#21556,#21557,#21558,#21559,#21560,
#21561,#21562,#21563,#21564,#21565,#21566,#21567,#21568,#21569,#21570,#21571,
#21572,#21573,#21574,#21575,#21576,#21577,#21578,#21579,#21580,#21581,#21582,
#21583,#21584,#21585,#21586,#21587,#21588,#21589,#21590,#21591,#21592,#21593,
#21594,#21595,#21596,#21597,#21598,#21599,#21600,#21601,#21602,#21603,#21604,
#21605,#21606,#21607,#21608,#21609,#21610,#21611,#21612,#21613,#21614,#21615,
#21616,#21617,#21618,#21619,#21620,#21621,#21622,#21623,#21624,#21625,#21626,
#21627,#21628,#21629,#21630,#21631,#21632,#21633,#21634,#21635,#21636,#21637,
#21638,#21639,#21640,#21641,#21642,#21643,#21644,#21645,#21646,#21647,#21648,
#21649,#21650,#21651,#21652,#21653,#21654,#21655,#21656,#21657,#21658,#21659,
#21660,#21661,#21662,#21663,#21664,#21665,#21666,#21667,#21668,#21669,#21670,
#21671,#21672,#21673,#21674,#21675,#21676,#21677,#21678,#21679,#21680,#21681,
#21682,#21683,#21684,#21685,#21686,#21687,#21688,#21689,#21690,#21691,#21692,
#21693,#21694,#21695,#21696,#21697,#21698,#21699,#21700,#21701,#21702,#21703,
#21704,#21705,#21706,#21707,#21708,#21709,#21710,#21711,#21712,#21713,#21714,
#21715,#21716,#21717,#21718,#21719,#21720,#21721,#21722,#21723,#21724,#21725,
#21726,#21727,#21728,#21729,#21730,#21731,#21732,#21733,#21734,#21735,#21736,
#21737,#21738,#21739,#21740,#21741,#21742,#21743,#21744,#21745,#21746,#21747,
#21748,#21749,#21750,#21751,#21752,#21753,#21754,#21755,#21756,#21757,#21758,
#21759,#21760,#21761,#21762,#21763,#21764),(#21765,#21766,#21767,#21768,
#21769,#21770,#21771,#21772,#21773,#21774,#21775,#21776,#21777,#21778,#21779,
#21780,#21781,#21782,#21783,#21784,#21785,#21786,#21787,#21788,#21789,#21790,
#21791,#21792,#21793,#21794,#21795,#21796,#21797,#21798,#21799,#21800,#21801,
#21802,#21803,#21804,#21805,#21806,#21807,#21808,#21809,#21810,#21811,#21812,
#21813,#21814,#21815,#21816,#21817,#21818,#21819,#21820,#21821,#21822,#21823,
#21824,#21825,#21826,#21827,#21828,#21829,#21830,#21831,#21832,#21833,#21834,
#21835,#21836,#21837,#21838,#21839,#21840,#21841,#21842,#21843,#21844,#21845,
#21846,#21847,#21848,#21849,#21850,#21851,#21852,#21853,#21854,#21855,#21856,
#21857,#21858,#21859,#21860,#21861,#21862,#21863,#21864,#21865,#21866,#21867,
#21868,#21869,#21870,#21871,#21872,#21873,#21874,#21875,#21876,#21877,#21878,
#21879,#21880,#21881,#21882,#21883,#21884,#21885,#21886,#21887,#21888,#21889,
#21890,#21891,#21892,#21893,#21894,#21895,#21896,#21897,#21898,#21899,#21900,
#21901,#21902,#21903,#21904,#21905,#21906,#21907,#21908,#21909,#21910,#21911,
#21912,#21913,#21914,#21915,#21916,#21917,#21918,#21919,#21920,#21921,#21922,
#21923,#21924,#21925,#21926,#21927,#21928,#21929,#21930,#21931,#21932,#21933,
#21934,#21935,#21936,#21937,#21938,#21939,#21940,#21941,#21942,#21943,#21944,
#21945,#21946,#21947,#21948,#21949,#21950,#21951,#21952,#21953,#21954,#21955,
#21956,#21957,#21958,#21959,#21960,#21961,#21962,#21963,#21964,#21965,#21966,
#21967,#21968,#21969,#21970,#21971,#21972,#21973,#21974,#21975,#21976,#21977,
#21978,#21979,#21980,#21981,#21982,#21983,#21984,#21985,#21986,#21987,#21988,
#21989,#21990,#21991,#21992,#21993,#21994,#21995,#21996,#21997,#21998,#21999,
#22000,#22001,#22002,#22003,#22004,#22005,#22006,#22007,#22008,#22009,#22010,
#22011,#22012,#22013,#22014,#22015,#22016,#22017,#22018,#22019,#22020,#22021,
#22022,#22023,#22024,#22025,#22026,#22027,#22028,#22029,#22030,#22031,#22032,
#22033,#22034,#22035,#22036,#22037,#22038,#22039,#22040,#22041,#22042,#22043,
#22044,#22045,#22046,#22047,#22048,#22049,#22050,#22051,#22052,#22053,#22054,
#22055,#22056,#22057,#22058,#22059,#22060,#22061,#22062,#22063,#22064,#22065,
#22066,#22067,#22068,#22069,#22070,#22071,#22072,#22073,#22074,#22075,#22076,
#22077,#22078,#22079,#22080,#22081,#22082,#22083,#22084,#22085,#22086,#22087,
#22088,#22089,#22090,#22091,#22092,#22093,#22094,#22095,#22096,#22097,#22098,
#22099,#22100,#22101,#22102,#22103,#22104,#22105,#22106,#22107,#22108,#22109,
#22110,#22111,#22112,#22113,#22114,#22115,#22116,#22117,#22118,#22119,#22120,
#22121,#22122,#22123,#22124,#22125,#22126,#22127,#22128,#22129,#22130,#22131,
#22132,#22133,#22134,#22135,#22136,#22137,#22138,#22139,#22140,#22141,#22142,
#22143,#22144,#22145,#22146,#22147,#22148,#22149,#22150,#22151,#22152,#22153,
#22154,#22155,#22156,#22157,#22158,#22159,#22160,#22161,#22162,#22163,#22164,
#22165,#22166,#22167,#22168,#22169,#22170,#22171,#22172,#22173,#22174,#22175,
#22176,#22177,#22178,#22179,#22180,#22181,#22182,#22183,#22184,#22185,#22186,
#22187,#22188,#22189,#22190,#22191,#22192,#22193,#22194,#22195,#22196,#22197,
#22198,#22199,#22200,#22201,#22202,#22203,#22204,#22205,#22206,#22207,#22208,
#22209,#22210,#22211,#22212,#22213,#22214,#22215,#22216,#22217,#22218,#22219,
#22220,#22221,#22222,#22223,#22224,#22225,#22226,#22227,#22228,#22229,#22230,
#22231,#22232,#22233,#22234,#22235,#22236,#22237,#22238,#22239,#22240,#22241,
#22242,#22243,#22244,#22245,#22246,#22247,#22248,#22249,#22250,#22251,#22252,
#22253,#22254,#22255,#22256,#22257,#22258,#22259,#22260,#22261,#22262)),
 .UNSPECIFIED.,.F.,.F.,.F.,(4,4),(4,1,1,1,1,1,1,1,1,1,1,1,1,1,1,1,1,1,1,
1,1,1,1,1,1,1,1,1,1,1,1,1,1,1,1,1,1,1,1,1,1,1,1,1,1,1,1,1,1,1,1,1,1,1,1,
1,1,1,1,1,1,1,1,1,1,1,1,1,1,1,1,1,1,1,1,1,1,1,1,1,1,1,1,1,1,1,1,1,1,1,1,
1,1,1,1,1,1,1,1,1,1,1,1,1,1,1,1,1,1,1,1,1,1,1,1,1,1,1,1,1,1,1,1,1,1,1,1,
1,1,1,1,1,1,1,1,1,1,1,1,1,1,1,1,1,1,1,1,1,1,1,1,1,1,1,1,1,1,1,1,1,1,1,1,
1,1,1,1,1,1,1,1,1,1,1,1,1,1,1,1,1,1,1,1,1,1,1,1,1,1,1,1,1,1,1,1,1,1,1,1,
1,1,1,1,1,1,1,1,1,1,1,1,1,1,1,1,1,1,1,1,1,1,1,1,1,1,1,1,1,1,1,1,1,1,1,1,
1,1,1,1,1,1,1,1,1,1,1,1,1,1,1,1,1,1,1,1,1,1,1,1,1,1,1,1,1,1,1,1,1,1,1,1,
1,1,1,1,1,1,1,1,1,1,1,1,1,1,1,1,1,1,1,1,1,1,1,1,1,1,1,1,1,1,1,1,1,1,1,1,
1,1,1,1,1,1,1,1,1,1,1,1,1,1,1,1,1,1,1,1,1,1,1,1,1,1,1,1,1,1,1,1,1,1,1,1,
1,1,1,1,1,1,1,1,1,1,1,1,1,1,1,1,1,1,1,1,1,1,1,1,1,1,1,1,1,1,1,1,1,1,1,1,
1,1,1,1,1,1,1,1,1,1,1,1,1,1,1,1,1,1,1,1,1,1,1,1,1,1,1,1,1,1,1,1,1,1,1,1,
1,1,1,1,1,1,1,1,1,1,1,1,1,1,1,1,1,1,1,1,1,1,1,1,1,1,1,1,1,1,1,1,1,1,1,1,
1,1,1,1,1,1,1,1,1,1,1,1,1,1,1,1,1,1,1,1,1,1,1,1,1,1,1,1,1,1,1,1,1,1,1,1,
1,1,1,1,1,1,1,1,4),(0.,0.184512097253587),(8.98171729021681,9.48139635699984,
9.98107542378286,10.4807544905659,10.9804335573489,11.4801126241319,11.979791690915,
12.479470757698,12.979149824481,13.478828891264,13.9785079580471,14.4781870248301,
14.9778660916131,15.4775451583961,15.9772242251791,16.4769032919622,16.9765823587452,
17.4762614255282,17.9759404923112,18.4756195590943,18.9752986258773,19.4749776926603,
19.9746567594433,20.4743358262264,20.9740148930094,21.4736939597924,21.9733730265754,
22.4730520933585,22.9727311601415,23.4724102269245,23.9720892937075,24.4717683604905,
24.9714474272736,25.4711264940566,25.9708055608396,26.4704846276226,26.9701636944057,
27.4698427611887,27.9695218279717,28.4692008947547,28.9688799615378,29.4685590283208,
29.9682380951038,30.4679171618868,30.9675962286699,31.4672752954529,31.9669543622359,
32.4666334290189,32.966312495802,33.465991562585,33.965670629368,34.465349696151,
34.965028762934,35.4647078297171,35.9643868965001,36.4640659632831,36.9637450300661,
37.4634240968492,37.9631031636322,38.4627822304152,38.9624612971982,39.4621403639813,
39.9618194307643,40.4614984975473,40.9611775643303,41.4608566311134,41.9605356978964,
42.4602147646794,42.9598938314624,43.4595728982454,43.9592519650285,44.4589310318115,
44.9586100985945,45.4582891653775,45.9579682321606,46.4576472989436,46.9573263657266,
47.4570054325096,47.9566844992927,48.4563635660757,48.9560426328587,49.4557216996417,
49.9554007664248,50.4550798332078,50.9547588999908,51.4544379667738,51.9541170335568,
52.4537961003399,52.9534751671229,53.4531542339059,53.9528333006889,54.452512367472,
54.952191434255,55.451870501038,55.951549567821,56.4512286346041,56.9509077013871,
57.4505867681701,57.9502658349531,58.4499449017362,58.9496239685192,59.9489821020852,
60.9483402356513,61.9476983692173,62.9470565027834,63.9464146363494,64.9457727699155,
65.9451309034815,66.9444890370476,67.9438471706136,68.9432053041797,69.9425634377457,
70.9419215713118,71.9412797048778,72.9406378384438,73.9399959720099,74.9393541055759,
75.938712239142,76.938070372708,77.9374285062741,78.9367866398401,79.9361447734062,
80.9355029069722,81.9348610405383,82.9342191741043,83.9335773076704,84.9329354412364,
85.9322935748025,86.9316517083685,87.9310098419346,88.9303679755006,89.9297261090666,
90.9290842426327,91.9284423761987,92.9278005097648,93.9271586433308,94.9265167768969,
95.9258749104629,96.925233044029,97.924591177595,98.9239493111611,99.9233074447271,
100.922665578293,101.922023711859,102.921381845425,103.920739978991,104.920098112557,
105.919456246123,106.918814379689,107.918172513255,108.917530646822,109.916888780388,
110.916246913954,111.91560504752,112.914963181086,113.914321314652,114.913679448218,
115.913037581784,116.91239571535,117.911753848916,118.911111982482,119.910470116048,
120.909828249614,121.90918638318,122.908544516746,123.907902650312,124.907260783878,
125.906618917444,126.90597705101,127.905335184576,128.904693318142,129.904051451709,
130.903409585275,131.902767718841,132.902125852407,133.901483985973,134.900842119539,
135.900200253105,136.899558386671,137.898916520237,138.898274653803,139.897632787369,
140.896990920935,141.896349054501,142.895707188067,143.895065321633,144.894423455199,
145.893781588765,146.893139722331,147.892497855897,148.891855989463,149.891214123029,
150.890572256596,151.889930390162,152.889288523728,153.888646657294,154.88800479086,
155.887362924426,156.886721057992,157.886079191558,158.885437325124,159.88479545869,
160.884153592256,161.883511725822,162.882869859388,163.882227992954,164.88158612652,
165.880944260086,166.880302393652,167.879660527218,168.879018660784,169.87837679435,
170.877734927916,171.877093061483,172.876451195049,173.875809328615,174.875167462181,
175.874525595747,176.873883729313,177.873241862879,178.872599996445,179.871958130011,
180.871316263577,181.870674397143,182.870032530709,183.869390664275,184.868748797841,
185.868106931407,186.867465064973,187.866823198539,188.866181332105,189.865539465671,
190.864897599237,191.864255732803,192.86361386637,193.862971999936,194.862330133502,
195.861688267068,196.861046400634,197.8604045342,198.859762667766,199.859120801332,
200.858478934898,201.857837068464,202.85719520203,203.856553335596,204.855911469162,
205.855269602728,206.854627736294,207.85398586986,208.853344003426,209.852702136992,
210.852060270558,211.851418404124,212.85077653769,213.850134671257,214.849492804823,
215.848850938389,216.848209071955,217.847567205521,218.846925339087,219.846283472653,
220.845641606219,221.844999739785,222.844357873351,223.843716006917,224.843074140483,
225.842432274049,226.841790407615,227.841148541181,228.840506674747,229.839864808313,
230.839222941879,231.838581075445,232.837939209011,233.837297342577,234.836655476144,
235.83601360971,236.835371743276,237.834729876842,238.834088010408,239.833446143974,
240.83280427754,241.832162411106,242.831520544672,243.830878678238,244.830236811804,
245.82959494537,246.828953078936,247.828311212502,248.827669346068,249.827027479634,
250.8263856132,251.825743746766,252.825101880332,253.824460013898,254.823818147464,
255.82317628103,256.822534414597,257.821892548163,258.821250681729,259.820608815295,
260.819966948861,261.819325082427,262.818683215993,263.818041349559,264.817399483125,
265.816757616691,266.816115750257,267.815473883823,268.814832017389,269.814190150955,
270.813548284521,271.812906418087,272.812264551653,273.811622685219,274.810980818785,
275.810338952351,276.809697085917,277.809055219484,278.80841335305,279.807771486616,
280.807129620182,281.806487753748,282.805845887314,283.80520402088,284.804562154446,
285.803920288012,286.803278421578,287.802636555144,288.80199468871,289.801352822276,
290.800710955842,291.800069089408,292.799427222974,293.79878535654,294.798143490106,
295.797501623672,296.796859757238,297.796217890804,298.795576024371,299.794934157937,
300.794292291503,301.793650425069,302.793008558635,303.792366692201,304.791724825767,
305.791082959333,306.790441092899,307.789799226465,308.789157360031,309.788515493597,
310.787873627163,311.787231760729,312.786589894295,313.785948027861,314.785306161427,
315.784664294993,316.784022428559,317.783380562125,318.782738695691,319.782096829258,
320.781454962824,321.78081309639,322.780171229956,323.779529363522,324.778887497088,
325.778245630654,326.77760376422,327.776961897786,328.776320031352,329.775678164918,
330.775036298484,331.77439443205,332.773752565616,333.773110699182,334.772468832748,
335.771826966314,336.77118509988,337.770543233446,338.769901367012,339.769259500578,
340.768617634145,341.767975767711,342.767333901277,343.766692034843,344.766050168409,
345.765408301975,346.764766435541,347.764124569107,348.763482702673,349.762840836239,
350.762198969805,351.761557103371,352.760915236937,353.760273370503,354.259952437286,
354.759631504069,355.259310570852,355.758989637635,356.258668704418,356.758347771201,
357.258026837984,357.757705904767,358.25738497155,358.757064038333,359.256743105116,
359.756422171899,360.256101238682,360.755780305465,361.255459372248,361.755138439031,
362.254817505815,362.754496572598,363.254175639381,363.753854706164,364.253533772947,
364.75321283973,365.252891906513,365.752570973296,366.252250040079,366.751929106862,
367.251608173645,367.751287240428,368.250966307211,368.750645373994,369.250324440777,
369.75000350756,370.249682574343,370.749361641126,371.249040707909,371.748719774692,
372.248398841475,372.748077908258,373.247756975041,373.747436041824,374.247115108607,
374.74679417539,375.246473242173,375.746152308956,376.245831375739,376.745510442522,
377.245189509305,377.744868576088,378.244547642871,378.744226709654,379.243905776437,
379.74358484322,380.243263910003,380.742942976786,381.242622043569,381.742301110352,
382.241980177135,382.741659243918,383.241338310702,383.741017377485,384.240696444268,
384.740375511051,385.240054577834,385.739733644617,386.2394127114,386.739091778183,
387.238770844966,387.738449911749,388.238128978532,388.737808045315,389.237487112098,
389.737166178881,390.236845245664,390.736524312447,391.23620337923,391.735882446013,
392.235561512796,392.735240579579,393.234919646362,393.734598713145,394.234277779928,
394.733956846711,395.233635913494,395.733314980277,396.23299404706,396.732673113843,
397.232352180626,397.732031247409,398.231710314192,398.731389380975,399.231068447758,
399.730747514541,400.230426581324,400.730105648107,401.22978471489,401.729463781673,
402.229142848456,402.728821915239,403.228500982022,403.728180048805),
 .UNSPECIFIED.);
#14=B_SPLINE_SURFACE_WITH_KNOTS('',3,3,((#22396,#22397,#22398,#22399,#22400,
#22401,#22402,#22403,#22404,#22405,#22406,#22407,#22408,#22409,#22410,#22411,
#22412,#22413,#22414,#22415,#22416,#22417,#22418,#22419,#22420,#22421,#22422,
#22423,#22424,#22425,#22426,#22427,#22428,#22429,#22430,#22431,#22432,#22433,
#22434,#22435,#22436,#22437,#22438,#22439,#22440,#22441,#22442,#22443,#22444,
#22445,#22446,#22447,#22448,#22449,#22450,#22451,#22452,#22453,#22454,#22455,
#22456,#22457,#22458,#22459,#22460,#22461,#22462,#22463,#22464,#22465,#22466,
#22467,#22468,#22469,#22470,#22471,#22472,#22473,#22474,#22475,#22476,#22477,
#22478,#22479,#22480,#22481,#22482,#22483,#22484,#22485,#22486,#22487,#22488,
#22489,#22490,#22491,#22492,#22493,#22494,#22495,#22496,#22497,#22498,#22499,
#22500,#22501,#22502,#22503,#22504,#22505,#22506,#22507,#22508,#22509,#22510,
#22511,#22512,#22513,#22514,#22515,#22516,#22517,#22518,#22519,#22520,#22521,
#22522,#22523,#22524,#22525,#22526,#22527,#22528,#22529,#22530,#22531,#22532,
#22533,#22534,#22535,#22536,#22537,#22538,#22539,#22540,#22541,#22542,#22543,
#22544,#22545,#22546,#22547,#22548,#22549,#22550,#22551,#22552,#22553,#22554,
#22555,#22556,#22557,#22558,#22559,#22560,#22561,#22562,#22563,#22564,#22565,
#22566,#22567,#22568,#22569,#22570,#22571,#22572,#22573,#22574,#22575,#22576,
#22577,#22578,#22579,#22580,#22581,#22582,#22583,#22584,#22585,#22586,#22587,
#22588,#22589,#22590,#22591,#22592,#22593,#22594,#22595,#22596,#22597,#22598,
#22599,#22600,#22601,#22602,#22603,#22604,#22605,#22606,#22607,#22608,#22609,
#22610,#22611,#22612,#22613,#22614,#22615,#22616,#22617,#22618,#22619,#22620,
#22621,#22622,#22623,#22624,#22625,#22626,#22627,#22628,#22629,#22630,#22631,
#22632,#22633,#22634,#22635,#22636,#22637,#22638,#22639,#22640,#22641,#22642,
#22643,#22644,#22645,#22646,#22647,#22648,#22649,#22650,#22651,#22652,#22653,
#22654,#22655,#22656,#22657,#22658,#22659,#22660,#22661,#22662,#22663,#22664,
#22665,#22666,#22667,#22668,#22669,#22670,#22671,#22672,#22673,#22674,#22675,
#22676,#22677,#22678,#22679,#22680,#22681,#22682,#22683,#22684,#22685,#22686,
#22687,#22688,#22689,#22690,#22691,#22692,#22693,#22694,#22695,#22696,#22697,
#22698,#22699,#22700,#22701,#22702,#22703,#22704,#22705,#22706,#22707,#22708,
#22709,#22710,#22711,#22712,#22713,#22714,#22715,#22716,#22717,#22718,#22719,
#22720,#22721,#22722,#22723,#22724,#22725,#22726,#22727,#22728,#22729,#22730,
#22731,#22732,#22733,#22734,#22735,#22736,#22737,#22738,#22739,#22740,#22741,
#22742,#22743,#22744,#22745,#22746,#22747,#22748,#22749,#22750,#22751,#22752,
#22753,#22754,#22755,#22756,#22757,#22758,#22759,#22760,#22761,#22762,#22763,
#22764,#22765,#22766,#22767,#22768,#22769,#22770,#22771,#22772,#22773,#22774,
#22775,#22776,#22777,#22778,#22779,#22780,#22781,#22782,#22783,#22784,#22785,
#22786,#22787,#22788,#22789,#22790,#22791,#22792,#22793,#22794,#22795,#22796,
#22797,#22798,#22799,#22800,#22801,#22802,#22803,#22804,#22805,#22806,#22807,
#22808,#22809,#22810,#22811,#22812,#22813,#22814,#22815,#22816,#22817,#22818,
#22819,#22820,#22821,#22822,#22823,#22824,#22825,#22826,#22827,#22828,#22829,
#22830,#22831,#22832,#22833,#22834,#22835,#22836,#22837,#22838,#22839,#22840,
#22841,#22842,#22843,#22844,#22845,#22846,#22847,#22848,#22849,#22850,#22851,
#22852,#22853,#22854,#22855,#22856,#22857,#22858,#22859,#22860,#22861,#22862,
#22863,#22864,#22865,#22866,#22867,#22868,#22869,#22870,#22871,#22872,#22873,
#22874,#22875,#22876,#22877,#22878,#22879,#22880,#22881,#22882,#22883,#22884,
#22885,#22886,#22887,#22888,#22889,#22890,#22891,#22892,#22893),(#22894,
#22895,#22896,#22897,#22898,#22899,#22900,#22901,#22902,#22903,#22904,#22905,
#22906,#22907,#22908,#22909,#22910,#22911,#22912,#22913,#22914,#22915,#22916,
#22917,#22918,#22919,#22920,#22921,#22922,#22923,#22924,#22925,#22926,#22927,
#22928,#22929,#22930,#22931,#22932,#22933,#22934,#22935,#22936,#22937,#22938,
#22939,#22940,#22941,#22942,#22943,#22944,#22945,#22946,#22947,#22948,#22949,
#22950,#22951,#22952,#22953,#22954,#22955,#22956,#22957,#22958,#22959,#22960,
#22961,#22962,#22963,#22964,#22965,#22966,#22967,#22968,#22969,#22970,#22971,
#22972,#22973,#22974,#22975,#22976,#22977,#22978,#22979,#22980,#22981,#22982,
#22983,#22984,#22985,#22986,#22987,#22988,#22989,#22990,#22991,#22992,#22993,
#22994,#22995,#22996,#22997,#22998,#22999,#23000,#23001,#23002,#23003,#23004,
#23005,#23006,#23007,#23008,#23009,#23010,#23011,#23012,#23013,#23014,#23015,
#23016,#23017,#23018,#23019,#23020,#23021,#23022,#23023,#23024,#23025,#23026,
#23027,#23028,#23029,#23030,#23031,#23032,#23033,#23034,#23035,#23036,#23037,
#23038,#23039,#23040,#23041,#23042,#23043,#23044,#23045,#23046,#23047,#23048,
#23049,#23050,#23051,#23052,#23053,#23054,#23055,#23056,#23057,#23058,#23059,
#23060,#23061,#23062,#23063,#23064,#23065,#23066,#23067,#23068,#23069,#23070,
#23071,#23072,#23073,#23074,#23075,#23076,#23077,#23078,#23079,#23080,#23081,
#23082,#23083,#23084,#23085,#23086,#23087,#23088,#23089,#23090,#23091,#23092,
#23093,#23094,#23095,#23096,#23097,#23098,#23099,#23100,#23101,#23102,#23103,
#23104,#23105,#23106,#23107,#23108,#23109,#23110,#23111,#23112,#23113,#23114,
#23115,#23116,#23117,#23118,#23119,#23120,#23121,#23122,#23123,#23124,#23125,
#23126,#23127,#23128,#23129,#23130,#23131,#23132,#23133,#23134,#23135,#23136,
#23137,#23138,#23139,#23140,#23141,#23142,#23143,#23144,#23145,#23146,#23147,
#23148,#23149,#23150,#23151,#23152,#23153,#23154,#23155,#23156,#23157,#23158,
#23159,#23160,#23161,#23162,#23163,#23164,#23165,#23166,#23167,#23168,#23169,
#23170,#23171,#23172,#23173,#23174,#23175,#23176,#23177,#23178,#23179,#23180,
#23181,#23182,#23183,#23184,#23185,#23186,#23187,#23188,#23189,#23190,#23191,
#23192,#23193,#23194,#23195,#23196,#23197,#23198,#23199,#23200,#23201,#23202,
#23203,#23204,#23205,#23206,#23207,#23208,#23209,#23210,#23211,#23212,#23213,
#23214,#23215,#23216,#23217,#23218,#23219,#23220,#23221,#23222,#23223,#23224,
#23225,#23226,#23227,#23228,#23229,#23230,#23231,#23232,#23233,#23234,#23235,
#23236,#23237,#23238,#23239,#23240,#23241,#23242,#23243,#23244,#23245,#23246,
#23247,#23248,#23249,#23250,#23251,#23252,#23253,#23254,#23255,#23256,#23257,
#23258,#23259,#23260,#23261,#23262,#23263,#23264,#23265,#23266,#23267,#23268,
#23269,#23270,#23271,#23272,#23273,#23274,#23275,#23276,#23277,#23278,#23279,
#23280,#23281,#23282,#23283,#23284,#23285,#23286,#23287,#23288,#23289,#23290,
#23291,#23292,#23293,#23294,#23295,#23296,#23297,#23298,#23299,#23300,#23301,
#23302,#23303,#23304,#23305,#23306,#23307,#23308,#23309,#23310,#23311,#23312,
#23313,#23314,#23315,#23316,#23317,#23318,#23319,#23320,#23321,#23322,#23323,
#23324,#23325,#23326,#23327,#23328,#23329,#23330,#23331,#23332,#23333,#23334,
#23335,#23336,#23337,#23338,#23339,#23340,#23341,#23342,#23343,#23344,#23345,
#23346,#23347,#23348,#23349,#23350,#23351,#23352,#23353,#23354,#23355,#23356,
#23357,#23358,#23359,#23360,#23361,#23362,#23363,#23364,#23365,#23366,#23367,
#23368,#23369,#23370,#23371,#23372,#23373,#23374,#23375,#23376,#23377,#23378,
#23379,#23380,#23381,#23382,#23383,#23384,#23385,#23386,#23387,#23388,#23389,
#23390,#23391),(#23392,#23393,#23394,#23395,#23396,#23397,#23398,#23399,
#23400,#23401,#23402,#23403,#23404,#23405,#23406,#23407,#23408,#23409,#23410,
#23411,#23412,#23413,#23414,#23415,#23416,#23417,#23418,#23419,#23420,#23421,
#23422,#23423,#23424,#23425,#23426,#23427,#23428,#23429,#23430,#23431,#23432,
#23433,#23434,#23435,#23436,#23437,#23438,#23439,#23440,#23441,#23442,#23443,
#23444,#23445,#23446,#23447,#23448,#23449,#23450,#23451,#23452,#23453,#23454,
#23455,#23456,#23457,#23458,#23459,#23460,#23461,#23462,#23463,#23464,#23465,
#23466,#23467,#23468,#23469,#23470,#23471,#23472,#23473,#23474,#23475,#23476,
#23477,#23478,#23479,#23480,#23481,#23482,#23483,#23484,#23485,#23486,#23487,
#23488,#23489,#23490,#23491,#23492,#23493,#23494,#23495,#23496,#23497,#23498,
#23499,#23500,#23501,#23502,#23503,#23504,#23505,#23506,#23507,#23508,#23509,
#23510,#23511,#23512,#23513,#23514,#23515,#23516,#23517,#23518,#23519,#23520,
#23521,#23522,#23523,#23524,#23525,#23526,#23527,#23528,#23529,#23530,#23531,
#23532,#23533,#23534,#23535,#23536,#23537,#23538,#23539,#23540,#23541,#23542,
#23543,#23544,#23545,#23546,#23547,#23548,#23549,#23550,#23551,#23552,#23553,
#23554,#23555,#23556,#23557,#23558,#23559,#23560,#23561,#23562,#23563,#23564,
#23565,#23566,#23567,#23568,#23569,#23570,#23571,#23572,#23573,#23574,#23575,
#23576,#23577,#23578,#23579,#23580,#23581,#23582,#23583,#23584,#23585,#23586,
#23587,#23588,#23589,#23590,#23591,#23592,#23593,#23594,#23595,#23596,#23597,
#23598,#23599,#23600,#23601,#23602,#23603,#23604,#23605,#23606,#23607,#23608,
#23609,#23610,#23611,#23612,#23613,#23614,#23615,#23616,#23617,#23618,#23619,
#23620,#23621,#23622,#23623,#23624,#23625,#23626,#23627,#23628,#23629,#23630,
#23631,#23632,#23633,#23634,#23635,#23636,#23637,#23638,#23639,#23640,#23641,
#23642,#23643,#23644,#23645,#23646,#23647,#23648,#23649,#23650,#23651,#23652,
#23653,#23654,#23655,#23656,#23657,#23658,#23659,#23660,#23661,#23662,#23663,
#23664,#23665,#23666,#23667,#23668,#23669,#23670,#23671,#23672,#23673,#23674,
#23675,#23676,#23677,#23678,#23679,#23680,#23681,#23682,#23683,#23684,#23685,
#23686,#23687,#23688,#23689,#23690,#23691,#23692,#23693,#23694,#23695,#23696,
#23697,#23698,#23699,#23700,#23701,#23702,#23703,#23704,#23705,#23706,#23707,
#23708,#23709,#23710,#23711,#23712,#23713,#23714,#23715,#23716,#23717,#23718,
#23719,#23720,#23721,#23722,#23723,#23724,#23725,#23726,#23727,#23728,#23729,
#23730,#23731,#23732,#23733,#23734,#23735,#23736,#23737,#23738,#23739,#23740,
#23741,#23742,#23743,#23744,#23745,#23746,#23747,#23748,#23749,#23750,#23751,
#23752,#23753,#23754,#23755,#23756,#23757,#23758,#23759,#23760,#23761,#23762,
#23763,#23764,#23765,#23766,#23767,#23768,#23769,#23770,#23771,#23772,#23773,
#23774,#23775,#23776,#23777,#23778,#23779,#23780,#23781,#23782,#23783,#23784,
#23785,#23786,#23787,#23788,#23789,#23790,#23791,#23792,#23793,#23794,#23795,
#23796,#23797,#23798,#23799,#23800,#23801,#23802,#23803,#23804,#23805,#23806,
#23807,#23808,#23809,#23810,#23811,#23812,#23813,#23814,#23815,#23816,#23817,
#23818,#23819,#23820,#23821,#23822,#23823,#23824,#23825,#23826,#23827,#23828,
#23829,#23830,#23831,#23832,#23833,#23834,#23835,#23836,#23837,#23838,#23839,
#23840,#23841,#23842,#23843,#23844,#23845,#23846,#23847,#23848,#23849,#23850,
#23851,#23852,#23853,#23854,#23855,#23856,#23857,#23858,#23859,#23860,#23861,
#23862,#23863,#23864,#23865,#23866,#23867,#23868,#23869,#23870,#23871,#23872,
#23873,#23874,#23875,#23876,#23877,#23878,#23879,#23880,#23881,#23882,#23883,
#23884,#23885,#23886,#23887,#23888,#23889),(#23890,#23891,#23892,#23893,
#23894,#23895,#23896,#23897,#23898,#23899,#23900,#23901,#23902,#23903,#23904,
#23905,#23906,#23907,#23908,#23909,#23910,#23911,#23912,#23913,#23914,#23915,
#23916,#23917,#23918,#23919,#23920,#23921,#23922,#23923,#23924,#23925,#23926,
#23927,#23928,#23929,#23930,#23931,#23932,#23933,#23934,#23935,#23936,#23937,
#23938,#23939,#23940,#23941,#23942,#23943,#23944,#23945,#23946,#23947,#23948,
#23949,#23950,#23951,#23952,#23953,#23954,#23955,#23956,#23957,#23958,#23959,
#23960,#23961,#23962,#23963,#23964,#23965,#23966,#23967,#23968,#23969,#23970,
#23971,#23972,#23973,#23974,#23975,#23976,#23977,#23978,#23979,#23980,#23981,
#23982,#23983,#23984,#23985,#23986,#23987,#23988,#23989,#23990,#23991,#23992,
#23993,#23994,#23995,#23996,#23997,#23998,#23999,#24000,#24001,#24002,#24003,
#24004,#24005,#24006,#24007,#24008,#24009,#24010,#24011,#24012,#24013,#24014,
#24015,#24016,#24017,#24018,#24019,#24020,#24021,#24022,#24023,#24024,#24025,
#24026,#24027,#24028,#24029,#24030,#24031,#24032,#24033,#24034,#24035,#24036,
#24037,#24038,#24039,#24040,#24041,#24042,#24043,#24044,#24045,#24046,#24047,
#24048,#24049,#24050,#24051,#24052,#24053,#24054,#24055,#24056,#24057,#24058,
#24059,#24060,#24061,#24062,#24063,#24064,#24065,#24066,#24067,#24068,#24069,
#24070,#24071,#24072,#24073,#24074,#24075,#24076,#24077,#24078,#24079,#24080,
#24081,#24082,#24083,#24084,#24085,#24086,#24087,#24088,#24089,#24090,#24091,
#24092,#24093,#24094,#24095,#24096,#24097,#24098,#24099,#24100,#24101,#24102,
#24103,#24104,#24105,#24106,#24107,#24108,#24109,#24110,#24111,#24112,#24113,
#24114,#24115,#24116,#24117,#24118,#24119,#24120,#24121,#24122,#24123,#24124,
#24125,#24126,#24127,#24128,#24129,#24130,#24131,#24132,#24133,#24134,#24135,
#24136,#24137,#24138,#24139,#24140,#24141,#24142,#24143,#24144,#24145,#24146,
#24147,#24148,#24149,#24150,#24151,#24152,#24153,#24154,#24155,#24156,#24157,
#24158,#24159,#24160,#24161,#24162,#24163,#24164,#24165,#24166,#24167,#24168,
#24169,#24170,#24171,#24172,#24173,#24174,#24175,#24176,#24177,#24178,#24179,
#24180,#24181,#24182,#24183,#24184,#24185,#24186,#24187,#24188,#24189,#24190,
#24191,#24192,#24193,#24194,#24195,#24196,#24197,#24198,#24199,#24200,#24201,
#24202,#24203,#24204,#24205,#24206,#24207,#24208,#24209,#24210,#24211,#24212,
#24213,#24214,#24215,#24216,#24217,#24218,#24219,#24220,#24221,#24222,#24223,
#24224,#24225,#24226,#24227,#24228,#24229,#24230,#24231,#24232,#24233,#24234,
#24235,#24236,#24237,#24238,#24239,#24240,#24241,#24242,#24243,#24244,#24245,
#24246,#24247,#24248,#24249,#24250,#24251,#24252,#24253,#24254,#24255,#24256,
#24257,#24258,#24259,#24260,#24261,#24262,#24263,#24264,#24265,#24266,#24267,
#24268,#24269,#24270,#24271,#24272,#24273,#24274,#24275,#24276,#24277,#24278,
#24279,#24280,#24281,#24282,#24283,#24284,#24285,#24286,#24287,#24288,#24289,
#24290,#24291,#24292,#24293,#24294,#24295,#24296,#24297,#24298,#24299,#24300,
#24301,#24302,#24303,#24304,#24305,#24306,#24307,#24308,#24309,#24310,#24311,
#24312,#24313,#24314,#24315,#24316,#24317,#24318,#24319,#24320,#24321,#24322,
#24323,#24324,#24325,#24326,#24327,#24328,#24329,#24330,#24331,#24332,#24333,
#24334,#24335,#24336,#24337,#24338,#24339,#24340,#24341,#24342,#24343,#24344,
#24345,#24346,#24347,#24348,#24349,#24350,#24351,#24352,#24353,#24354,#24355,
#24356,#24357,#24358,#24359,#24360,#24361,#24362,#24363,#24364,#24365,#24366,
#24367,#24368,#24369,#24370,#24371,#24372,#24373,#24374,#24375,#24376,#24377,
#24378,#24379,#24380,#24381,#24382,#24383,#24384,#24385,#24386,#24387)),
 .UNSPECIFIED.,.F.,.F.,.F.,(4,4),(4,1,1,1,1,1,1,1,1,1,1,1,1,1,1,1,1,1,1,
1,1,1,1,1,1,1,1,1,1,1,1,1,1,1,1,1,1,1,1,1,1,1,1,1,1,1,1,1,1,1,1,1,1,1,1,
1,1,1,1,1,1,1,1,1,1,1,1,1,1,1,1,1,1,1,1,1,1,1,1,1,1,1,1,1,1,1,1,1,1,1,1,
1,1,1,1,1,1,1,1,1,1,1,1,1,1,1,1,1,1,1,1,1,1,1,1,1,1,1,1,1,1,1,1,1,1,1,1,
1,1,1,1,1,1,1,1,1,1,1,1,1,1,1,1,1,1,1,1,1,1,1,1,1,1,1,1,1,1,1,1,1,1,1,1,
1,1,1,1,1,1,1,1,1,1,1,1,1,1,1,1,1,1,1,1,1,1,1,1,1,1,1,1,1,1,1,1,1,1,1,1,
1,1,1,1,1,1,1,1,1,1,1,1,1,1,1,1,1,1,1,1,1,1,1,1,1,1,1,1,1,1,1,1,1,1,1,1,
1,1,1,1,1,1,1,1,1,1,1,1,1,1,1,1,1,1,1,1,1,1,1,1,1,1,1,1,1,1,1,1,1,1,1,1,
1,1,1,1,1,1,1,1,1,1,1,1,1,1,1,1,1,1,1,1,1,1,1,1,1,1,1,1,1,1,1,1,1,1,1,1,
1,1,1,1,1,1,1,1,1,1,1,1,1,1,1,1,1,1,1,1,1,1,1,1,1,1,1,1,1,1,1,1,1,1,1,1,
1,1,1,1,1,1,1,1,1,1,1,1,1,1,1,1,1,1,1,1,1,1,1,1,1,1,1,1,1,1,1,1,1,1,1,1,
1,1,1,1,1,1,1,1,1,1,1,1,1,1,1,1,1,1,1,1,1,1,1,1,1,1,1,1,1,1,1,1,1,1,1,1,
1,1,1,1,1,1,1,1,1,1,1,1,1,1,1,1,1,1,1,1,1,1,1,1,1,1,1,1,1,1,1,1,1,1,1,1,
1,1,1,1,1,1,1,1,1,1,1,1,1,1,1,1,1,1,1,1,1,1,1,1,1,1,1,1,1,1,1,1,1,1,1,1,
1,1,1,1,1,1,1,1,4),(0.,0.184512097253587),(12.0092477762453,12.5089268430284,
13.0086059098114,13.5082849765944,14.0079640433774,14.5076431101605,15.0073221769435,
15.5070012437265,16.0066803105095,16.5063593772925,17.0060384440756,17.5057175108586,
18.0053965776416,18.5050756444246,19.0047547112077,19.5044337779907,20.0041128447737,
20.5037919115567,21.0034709783398,21.5031500451228,22.0028291119058,22.5025081786888,
23.0021872454719,23.5018663122549,24.0015453790379,24.5012244458209,25.0009035126039,
25.500582579387,26.00026164617,26.499940712953,26.999619779736,27.4992988465191,
27.9989779133021,28.4986569800851,28.9983360468681,29.4980151136512,29.9976941804342,
30.4973732472172,30.9970523140002,31.4967313807832,31.9964104475663,32.4960895143493,
32.9957685811323,33.4954476479153,33.9951267146984,34.4948057814814,34.9944848482644,
35.4941639150474,35.9938429818305,36.4935220486135,36.9932011153965,37.4928801821795,
37.9925592489626,38.4922383157456,38.9919173825286,39.4915964493116,39.9912755160946,
40.4909545828777,40.9906336496607,41.4903127164437,41.9899917832267,42.4896708500098,
42.9893499167928,43.4890289835758,43.9887080503588,44.4883871171419,44.9880661839249,
45.4877452507079,45.9874243174909,46.4871033842739,46.986782451057,47.48646151784,
47.986140584623,48.485819651406,48.9854987181891,49.4851777849721,49.9848568517551,
50.4845359185381,50.9842149853212,51.4838940521042,51.9835731188872,52.4832521856702,
52.9829312524532,53.4826103192363,53.9822893860193,54.4819684528023,54.9816475195853,
55.4813265863684,55.9810056531514,56.4806847199344,56.9803637867174,57.4800428535005,
57.9797219202835,58.4794009870665,58.9790800538495,59.4787591206325,59.9784381874156,
60.4781172541986,60.9777963209816,61.4774753877646,61.9771544545477,62.9765125881137,
63.9758707216798,64.9752288552458,65.9745869888119,66.9739451223779,67.9733032559439,
68.97266138951,69.972019523076,70.9713776566421,71.9707357902081,72.9700939237742,
73.9694520573402,74.9688101909063,75.9681683244723,76.9675264580384,77.9668845916044,
78.9662427251705,79.9656008587365,80.9649589923026,81.9643171258686,82.9636752594347,
83.9630333930007,84.9623915265667,85.9617496601328,86.9611077936988,87.9604659272649,
88.9598240608309,89.959182194397,90.958540327963,91.9578984615291,92.9572565950951,
93.9566147286612,94.9559728622272,95.9553309957932,96.9546891293593,97.9540472629253,
98.9534053964914,99.9527635300574,100.952121663623,101.95147979719,102.950837930756,
103.950196064322,104.949554197888,105.948912331454,106.94827046502,107.947628598586,
108.946986732152,109.946344865718,110.945702999284,111.94506113285,112.944419266416,
113.943777399982,114.943135533548,115.942493667114,116.94185180068,117.941209934246,
118.940568067812,119.939926201378,120.939284334944,121.93864246851,122.938000602077,
123.937358735643,124.936716869209,125.936075002775,126.935433136341,127.934791269907,
128.934149403473,129.933507537039,130.932865670605,131.932223804171,132.931581937737,
133.930940071303,134.930298204869,135.929656338435,136.929014472001,137.928372605567,
138.927730739133,139.927088872699,140.926447006265,141.925805139831,142.925163273397,
143.924521406963,144.92387954053,145.923237674096,146.922595807662,147.921953941228,
148.921312074794,149.92067020836,150.920028341926,151.919386475492,152.918744609058,
153.918102742624,154.91746087619,155.916819009756,156.916177143322,157.915535276888,
158.914893410454,159.91425154402,160.913609677586,161.912967811152,162.912325944718,
163.911684078284,164.91104221185,165.910400345416,166.909758478983,167.909116612549,
168.908474746115,169.907832879681,170.907191013247,171.906549146813,172.905907280379,
173.905265413945,174.904623547511,175.903981681077,176.903339814643,177.902697948209,
178.902056081775,179.901414215341,180.900772348907,181.900130482473,182.899488616039,
183.898846749605,184.898204883171,185.897563016737,186.896921150303,187.89627928387,
188.895637417436,189.894995551002,190.894353684568,191.893711818134,192.8930699517,
193.892428085266,194.891786218832,195.891144352398,196.890502485964,197.88986061953,
198.889218753096,199.888576886662,200.887935020228,201.887293153794,202.88665128736,
203.886009420926,204.885367554492,205.884725688058,206.884083821624,207.88344195519,
208.882800088756,209.882158222323,210.881516355889,211.880874489455,212.880232623021,
213.879590756587,214.878948890153,215.878307023719,216.877665157285,217.877023290851,
218.876381424417,219.875739557983,220.875097691549,221.874455825115,222.873813958681,
223.873172092247,224.872530225813,225.871888359379,226.871246492945,227.870604626511,
228.869962760077,229.869320893643,230.86867902721,231.868037160776,232.867395294342,
233.866753427908,234.866111561474,235.86546969504,236.864827828606,237.864185962172,
238.863544095738,239.862902229304,240.86226036287,241.861618496436,242.860976630002,
243.860334763568,244.859692897134,245.8590510307,246.858409164266,247.857767297832,
248.857125431398,249.856483564964,250.85584169853,251.855199832097,252.854557965663,
253.853916099229,254.853274232795,255.852632366361,256.851990499927,257.851348633493,
258.850706767059,259.850064900625,260.849423034191,261.848781167757,262.848139301323,
263.847497434889,264.846855568455,265.846213702021,266.845571835587,267.844929969153,
268.844288102719,269.843646236285,270.843004369851,271.842362503417,272.841720636983,
273.84107877055,274.840436904116,275.839795037682,276.839153171248,277.838511304814,
278.83786943838,279.837227571946,280.836585705512,281.835943839078,282.835301972644,
283.83466010621,284.834018239776,285.833376373342,286.832734506908,287.832092640474,
288.83145077404,289.830808907606,290.830167041172,291.829525174738,292.828883308304,
293.82824144187,294.827599575437,295.826957709003,296.826315842569,297.825673976135,
298.825032109701,299.824390243267,300.823748376833,301.823106510399,302.822464643965,
303.821822777531,304.821180911097,305.820539044663,306.819897178229,307.819255311795,
308.818613445361,309.817971578927,310.817329712493,311.816687846059,312.816045979625,
313.815404113191,314.814762246757,315.814120380323,316.81347851389,317.812836647456,
318.812194781022,319.811552914588,320.810911048154,321.81026918172,322.809627315286,
323.808985448852,324.808343582418,325.807701715984,326.80705984955,327.806417983116,
328.805776116682,329.805134250248,330.804492383814,331.80385051738,332.803208650946,
333.802566784512,334.801924918078,335.801283051644,336.80064118521,337.799999318776,
338.799357452343,339.798715585909,340.798073719475,341.797431853041,342.796789986607,
343.796148120173,344.795506253739,345.794864387305,346.794222520871,347.793580654437,
348.792938788003,349.792296921569,350.791655055135,351.791013188701,352.790371322267,
353.789729455833,354.789087589399,355.788445722965,356.787803856531,357.287482923314,
357.787161990097,358.28684105688,358.786520123663,359.286199190446,359.78587825723,
360.285557324013,360.785236390796,361.284915457579,361.784594524362,362.284273591145,
362.783952657928,363.283631724711,363.783310791494,364.282989858277,364.78266892506,
365.282347991843,365.782027058626,366.281706125409,366.781385192192,367.281064258975,
367.780743325758,368.280422392541,368.780101459324,369.279780526107,369.77945959289,
370.279138659673,370.778817726456,371.278496793239,371.778175860022,372.277854926805,
372.777533993588,373.277213060371,373.776892127154,374.276571193937,374.77625026072,
375.275929327503,375.775608394286,376.275287461069,376.774966527852,377.274645594635,
377.774324661418,378.274003728201,378.773682794984,379.273361861767,379.77304092855,
380.272719995333,380.772399062117,381.2720781289,381.771757195683,382.271436262466,
382.771115329249,383.270794396032,383.770473462815,384.270152529598,384.769831596381,
385.269510663164,385.769189729947,386.26886879673,386.768547863513,387.268226930296,
387.767905997079,388.267585063862,388.767264130645,389.266943197428,389.766622264211,
390.266301330994,390.765980397777,391.26565946456,391.765338531343,392.265017598126,
392.764696664909,393.264375731692,393.764054798475,394.263733865258,394.763412932041,
395.263091998824,395.762771065607,396.26245013239,396.762129199173,397.261808265956,
397.761487332739,398.261166399522,398.760845466305,399.260524533088,399.760203599871,
400.259882666654,400.759561733437,401.25924080022,401.758919867003,402.258598933787,
402.75827800057,403.257957067353,403.757636134136,404.257315200919,404.756994267702,
405.256673334485,405.756352401268,406.256031468051,406.755710534834),
 .UNSPECIFIED.);
#15=ITEM_DEFINED_TRANSFORMATION($,$,#8573,#8701);
#16=ITEM_DEFINED_TRANSFORMATION($,$,#8593,#8702);
#17=ITEM_DEFINED_TRANSFORMATION($,$,#8613,#8703);
#18=ITEM_DEFINED_TRANSFORMATION($,$,#8630,#8704);
#19=ITEM_DEFINED_TRANSFORMATION($,$,#8684,#8705);
#20=ITEM_DEFINED_TRANSFORMATION($,$,#8707,#8880);
#21=ITEM_DEFINED_TRANSFORMATION($,$,#8755,#8881);
#22=ITEM_DEFINED_TRANSFORMATION($,$,#8762,#8882);
#23=ITEM_DEFINED_TRANSFORMATION($,$,#8783,#8883);
#24=ITEM_DEFINED_TRANSFORMATION($,$,#8828,#8884);
#25=ITEM_DEFINED_TRANSFORMATION($,$,#8828,#8885);
#26=ITEM_DEFINED_TRANSFORMATION($,$,#8828,#8886);
#27=ITEM_DEFINED_TRANSFORMATION($,$,#8828,#8887);
#28=ITEM_DEFINED_TRANSFORMATION($,$,#8854,#8888);
#29=ITEM_DEFINED_TRANSFORMATION($,$,#8854,#8889);
#30=ITEM_DEFINED_TRANSFORMATION($,$,#8854,#8890);
#31=ITEM_DEFINED_TRANSFORMATION($,$,#8403,#9171);
#32=ITEM_DEFINED_TRANSFORMATION($,$,#8431,#9172);
#33=ITEM_DEFINED_TRANSFORMATION($,$,#8450,#9173);
#34=ITEM_DEFINED_TRANSFORMATION($,$,#8473,#9174);
#35=ITEM_DEFINED_TRANSFORMATION($,$,#8504,#9175);
#36=ITEM_DEFINED_TRANSFORMATION($,$,#8527,#9176);
#37=ITEM_DEFINED_TRANSFORMATION($,$,#8548,#9177);
#38=ITEM_DEFINED_TRANSFORMATION($,$,#8548,#9178);
#39=ITEM_DEFINED_TRANSFORMATION($,$,#8548,#9179);
#40=ITEM_DEFINED_TRANSFORMATION($,$,#9145,#9180);
#41=ITEM_DEFINED_TRANSFORMATION($,$,#9145,#9181);
#42=ITEM_DEFINED_TRANSFORMATION($,$,#9145,#9182);
#43=ITEM_DEFINED_TRANSFORMATION($,$,#9145,#9183);
#44=ITEM_DEFINED_TRANSFORMATION($,$,#8572,#9184);
#45=ITEM_DEFINED_TRANSFORMATION($,$,#8854,#9185);
#46=ITEM_DEFINED_TRANSFORMATION($,$,#8854,#9186);
#47=ITEM_DEFINED_TRANSFORMATION($,$,#8854,#9187);
#48=ITEM_DEFINED_TRANSFORMATION($,$,#8828,#9188);
#49=ITEM_DEFINED_TRANSFORMATION($,$,#8828,#9189);
#50=ITEM_DEFINED_TRANSFORMATION($,$,#8892,#9190);
#51=ITEM_DEFINED_TRANSFORMATION($,$,#9043,#9191);
#52=ITEM_DEFINED_TRANSFORMATION($,$,#9052,#9192);
#53=ITEM_DEFINED_TRANSFORMATION($,$,#9066,#9193);
#54=ITEM_DEFINED_TRANSFORMATION($,$,#9090,#9194);
#55=ITEM_DEFINED_TRANSFORMATION($,$,#9099,#9195);
#56=ITEM_DEFINED_TRANSFORMATION($,$,#9119,#9196);
#57=ITEM_DEFINED_TRANSFORMATION($,$,#9108,#9197);
#58=ITEM_DEFINED_TRANSFORMATION($,$,#9119,#9198);
#59=ITEM_DEFINED_TRANSFORMATION($,$,#9136,#9199);
#60=ITEM_DEFINED_TRANSFORMATION($,$,#9145,#9200);
#61=ITEM_DEFINED_TRANSFORMATION($,$,#8402,#9201);
#62=ITEM_DEFINED_TRANSFORMATION($,$,#8706,#9202);
#63=ITEM_DEFINED_TRANSFORMATION($,$,#8891,#9203);
#64=(
REPRESENTATION_RELATIONSHIP($,$,#25204,#25203)
REPRESENTATION_RELATIONSHIP_WITH_TRANSFORMATION(#15)
SHAPE_REPRESENTATION_RELATIONSHIP()
);
#65=(
REPRESENTATION_RELATIONSHIP($,$,#25205,#25203)
REPRESENTATION_RELATIONSHIP_WITH_TRANSFORMATION(#16)
SHAPE_REPRESENTATION_RELATIONSHIP()
);
#66=(
REPRESENTATION_RELATIONSHIP($,$,#25206,#25203)
REPRESENTATION_RELATIONSHIP_WITH_TRANSFORMATION(#17)
SHAPE_REPRESENTATION_RELATIONSHIP()
);
#67=(
REPRESENTATION_RELATIONSHIP($,$,#25207,#25203)
REPRESENTATION_RELATIONSHIP_WITH_TRANSFORMATION(#18)
SHAPE_REPRESENTATION_RELATIONSHIP()
);
#68=(
REPRESENTATION_RELATIONSHIP($,$,#25208,#25203)
REPRESENTATION_RELATIONSHIP_WITH_TRANSFORMATION(#19)
SHAPE_REPRESENTATION_RELATIONSHIP()
);
#69=(
REPRESENTATION_RELATIONSHIP($,$,#25210,#25209)
REPRESENTATION_RELATIONSHIP_WITH_TRANSFORMATION(#20)
SHAPE_REPRESENTATION_RELATIONSHIP()
);
#70=(
REPRESENTATION_RELATIONSHIP($,$,#25211,#25209)
REPRESENTATION_RELATIONSHIP_WITH_TRANSFORMATION(#21)
SHAPE_REPRESENTATION_RELATIONSHIP()
);
#71=(
REPRESENTATION_RELATIONSHIP($,$,#25212,#25209)
REPRESENTATION_RELATIONSHIP_WITH_TRANSFORMATION(#22)
SHAPE_REPRESENTATION_RELATIONSHIP()
);
#72=(
REPRESENTATION_RELATIONSHIP($,$,#25213,#25209)
REPRESENTATION_RELATIONSHIP_WITH_TRANSFORMATION(#23)
SHAPE_REPRESENTATION_RELATIONSHIP()
);
#73=(
REPRESENTATION_RELATIONSHIP($,$,#25214,#25209)
REPRESENTATION_RELATIONSHIP_WITH_TRANSFORMATION(#24)
SHAPE_REPRESENTATION_RELATIONSHIP()
);
#74=(
REPRESENTATION_RELATIONSHIP($,$,#25214,#25209)
REPRESENTATION_RELATIONSHIP_WITH_TRANSFORMATION(#25)
SHAPE_REPRESENTATION_RELATIONSHIP()
);
#75=(
REPRESENTATION_RELATIONSHIP($,$,#25214,#25209)
REPRESENTATION_RELATIONSHIP_WITH_TRANSFORMATION(#26)
SHAPE_REPRESENTATION_RELATIONSHIP()
);
#76=(
REPRESENTATION_RELATIONSHIP($,$,#25214,#25209)
REPRESENTATION_RELATIONSHIP_WITH_TRANSFORMATION(#27)
SHAPE_REPRESENTATION_RELATIONSHIP()
);
#77=(
REPRESENTATION_RELATIONSHIP($,$,#25215,#25209)
REPRESENTATION_RELATIONSHIP_WITH_TRANSFORMATION(#28)
SHAPE_REPRESENTATION_RELATIONSHIP()
);
#78=(
REPRESENTATION_RELATIONSHIP($,$,#25215,#25209)
REPRESENTATION_RELATIONSHIP_WITH_TRANSFORMATION(#29)
SHAPE_REPRESENTATION_RELATIONSHIP()
);
#79=(
REPRESENTATION_RELATIONSHIP($,$,#25215,#25209)
REPRESENTATION_RELATIONSHIP_WITH_TRANSFORMATION(#30)
SHAPE_REPRESENTATION_RELATIONSHIP()
);
#80=(
REPRESENTATION_RELATIONSHIP($,$,#25196,#25195)
REPRESENTATION_RELATIONSHIP_WITH_TRANSFORMATION(#31)
SHAPE_REPRESENTATION_RELATIONSHIP()
);
#81=(
REPRESENTATION_RELATIONSHIP($,$,#25197,#25195)
REPRESENTATION_RELATIONSHIP_WITH_TRANSFORMATION(#32)
SHAPE_REPRESENTATION_RELATIONSHIP()
);
#82=(
REPRESENTATION_RELATIONSHIP($,$,#25198,#25195)
REPRESENTATION_RELATIONSHIP_WITH_TRANSFORMATION(#33)
SHAPE_REPRESENTATION_RELATIONSHIP()
);
#83=(
REPRESENTATION_RELATIONSHIP($,$,#25199,#25195)
REPRESENTATION_RELATIONSHIP_WITH_TRANSFORMATION(#34)
SHAPE_REPRESENTATION_RELATIONSHIP()
);
#84=(
REPRESENTATION_RELATIONSHIP($,$,#25200,#25195)
REPRESENTATION_RELATIONSHIP_WITH_TRANSFORMATION(#35)
SHAPE_REPRESENTATION_RELATIONSHIP()
);
#85=(
REPRESENTATION_RELATIONSHIP($,$,#25201,#25195)
REPRESENTATION_RELATIONSHIP_WITH_TRANSFORMATION(#36)
SHAPE_REPRESENTATION_RELATIONSHIP()
);
#86=(
REPRESENTATION_RELATIONSHIP($,$,#25202,#25195)
REPRESENTATION_RELATIONSHIP_WITH_TRANSFORMATION(#37)
SHAPE_REPRESENTATION_RELATIONSHIP()
);
#87=(
REPRESENTATION_RELATIONSHIP($,$,#25202,#25195)
REPRESENTATION_RELATIONSHIP_WITH_TRANSFORMATION(#38)
SHAPE_REPRESENTATION_RELATIONSHIP()
);
#88=(
REPRESENTATION_RELATIONSHIP($,$,#25202,#25195)
REPRESENTATION_RELATIONSHIP_WITH_TRANSFORMATION(#39)
SHAPE_REPRESENTATION_RELATIONSHIP()
);
#89=(
REPRESENTATION_RELATIONSHIP($,$,#25226,#25195)
REPRESENTATION_RELATIONSHIP_WITH_TRANSFORMATION(#40)
SHAPE_REPRESENTATION_RELATIONSHIP()
);
#90=(
REPRESENTATION_RELATIONSHIP($,$,#25226,#25195)
REPRESENTATION_RELATIONSHIP_WITH_TRANSFORMATION(#41)
SHAPE_REPRESENTATION_RELATIONSHIP()
);
#91=(
REPRESENTATION_RELATIONSHIP($,$,#25226,#25195)
REPRESENTATION_RELATIONSHIP_WITH_TRANSFORMATION(#42)
SHAPE_REPRESENTATION_RELATIONSHIP()
);
#92=(
REPRESENTATION_RELATIONSHIP($,$,#25226,#25195)
REPRESENTATION_RELATIONSHIP_WITH_TRANSFORMATION(#43)
SHAPE_REPRESENTATION_RELATIONSHIP()
);
#93=(
REPRESENTATION_RELATIONSHIP($,$,#25203,#25195)
REPRESENTATION_RELATIONSHIP_WITH_TRANSFORMATION(#44)
SHAPE_REPRESENTATION_RELATIONSHIP()
);
#94=(
REPRESENTATION_RELATIONSHIP($,$,#25215,#25195)
REPRESENTATION_RELATIONSHIP_WITH_TRANSFORMATION(#45)
SHAPE_REPRESENTATION_RELATIONSHIP()
);
#95=(
REPRESENTATION_RELATIONSHIP($,$,#25215,#25195)
REPRESENTATION_RELATIONSHIP_WITH_TRANSFORMATION(#46)
SHAPE_REPRESENTATION_RELATIONSHIP()
);
#96=(
REPRESENTATION_RELATIONSHIP($,$,#25215,#25195)
REPRESENTATION_RELATIONSHIP_WITH_TRANSFORMATION(#47)
SHAPE_REPRESENTATION_RELATIONSHIP()
);
#97=(
REPRESENTATION_RELATIONSHIP($,$,#25214,#25195)
REPRESENTATION_RELATIONSHIP_WITH_TRANSFORMATION(#48)
SHAPE_REPRESENTATION_RELATIONSHIP()
);
#98=(
REPRESENTATION_RELATIONSHIP($,$,#25214,#25195)
REPRESENTATION_RELATIONSHIP_WITH_TRANSFORMATION(#49)
SHAPE_REPRESENTATION_RELATIONSHIP()
);
#99=(
REPRESENTATION_RELATIONSHIP($,$,#25217,#25216)
REPRESENTATION_RELATIONSHIP_WITH_TRANSFORMATION(#50)
SHAPE_REPRESENTATION_RELATIONSHIP()
);
#100=(
REPRESENTATION_RELATIONSHIP($,$,#25218,#25216)
REPRESENTATION_RELATIONSHIP_WITH_TRANSFORMATION(#51)
SHAPE_REPRESENTATION_RELATIONSHIP()
);
#101=(
REPRESENTATION_RELATIONSHIP($,$,#25219,#25216)
REPRESENTATION_RELATIONSHIP_WITH_TRANSFORMATION(#52)
SHAPE_REPRESENTATION_RELATIONSHIP()
);
#102=(
REPRESENTATION_RELATIONSHIP($,$,#25220,#25216)
REPRESENTATION_RELATIONSHIP_WITH_TRANSFORMATION(#53)
SHAPE_REPRESENTATION_RELATIONSHIP()
);
#103=(
REPRESENTATION_RELATIONSHIP($,$,#25221,#25216)
REPRESENTATION_RELATIONSHIP_WITH_TRANSFORMATION(#54)
SHAPE_REPRESENTATION_RELATIONSHIP()
);
#104=(
REPRESENTATION_RELATIONSHIP($,$,#25222,#25216)
REPRESENTATION_RELATIONSHIP_WITH_TRANSFORMATION(#55)
SHAPE_REPRESENTATION_RELATIONSHIP()
);
#105=(
REPRESENTATION_RELATIONSHIP($,$,#25224,#25216)
REPRESENTATION_RELATIONSHIP_WITH_TRANSFORMATION(#56)
SHAPE_REPRESENTATION_RELATIONSHIP()
);
#106=(
REPRESENTATION_RELATIONSHIP($,$,#25223,#25216)
REPRESENTATION_RELATIONSHIP_WITH_TRANSFORMATION(#57)
SHAPE_REPRESENTATION_RELATIONSHIP()
);
#107=(
REPRESENTATION_RELATIONSHIP($,$,#25224,#25216)
REPRESENTATION_RELATIONSHIP_WITH_TRANSFORMATION(#58)
SHAPE_REPRESENTATION_RELATIONSHIP()
);
#108=(
REPRESENTATION_RELATIONSHIP($,$,#25225,#25216)
REPRESENTATION_RELATIONSHIP_WITH_TRANSFORMATION(#59)
SHAPE_REPRESENTATION_RELATIONSHIP()
);
#109=(
REPRESENTATION_RELATIONSHIP($,$,#25226,#25216)
REPRESENTATION_RELATIONSHIP_WITH_TRANSFORMATION(#60)
SHAPE_REPRESENTATION_RELATIONSHIP()
);
#110=(
REPRESENTATION_RELATIONSHIP($,$,#25195,#25194)
REPRESENTATION_RELATIONSHIP_WITH_TRANSFORMATION(#61)
SHAPE_REPRESENTATION_RELATIONSHIP()
);
#111=(
REPRESENTATION_RELATIONSHIP($,$,#25209,#25194)
REPRESENTATION_RELATIONSHIP_WITH_TRANSFORMATION(#62)
SHAPE_REPRESENTATION_RELATIONSHIP()
);
#112=(
REPRESENTATION_RELATIONSHIP($,$,#25216,#25194)
REPRESENTATION_RELATIONSHIP_WITH_TRANSFORMATION(#63)
SHAPE_REPRESENTATION_RELATIONSHIP()
);
#113=CONTEXT_DEPENDENT_SHAPE_REPRESENTATION(#64,#25127);
#114=CONTEXT_DEPENDENT_SHAPE_REPRESENTATION(#65,#25128);
#115=CONTEXT_DEPENDENT_SHAPE_REPRESENTATION(#66,#25129);
#116=CONTEXT_DEPENDENT_SHAPE_REPRESENTATION(#67,#25130);
#117=CONTEXT_DEPENDENT_SHAPE_REPRESENTATION(#68,#25131);
#118=CONTEXT_DEPENDENT_SHAPE_REPRESENTATION(#69,#25139);
#119=CONTEXT_DEPENDENT_SHAPE_REPRESENTATION(#70,#25140);
#120=CONTEXT_DEPENDENT_SHAPE_REPRESENTATION(#71,#25141);
#121=CONTEXT_DEPENDENT_SHAPE_REPRESENTATION(#72,#25142);
#122=CONTEXT_DEPENDENT_SHAPE_REPRESENTATION(#73,#25143);
#123=CONTEXT_DEPENDENT_SHAPE_REPRESENTATION(#74,#25144);
#124=CONTEXT_DEPENDENT_SHAPE_REPRESENTATION(#75,#25145);
#125=CONTEXT_DEPENDENT_SHAPE_REPRESENTATION(#76,#25146);
#126=CONTEXT_DEPENDENT_SHAPE_REPRESENTATION(#77,#25147);
#127=CONTEXT_DEPENDENT_SHAPE_REPRESENTATION(#78,#25148);
#128=CONTEXT_DEPENDENT_SHAPE_REPRESENTATION(#79,#25149);
#129=CONTEXT_DEPENDENT_SHAPE_REPRESENTATION(#80,#25161);
#130=CONTEXT_DEPENDENT_SHAPE_REPRESENTATION(#81,#25162);
#131=CONTEXT_DEPENDENT_SHAPE_REPRESENTATION(#82,#25163);
#132=CONTEXT_DEPENDENT_SHAPE_REPRESENTATION(#83,#25164);
#133=CONTEXT_DEPENDENT_SHAPE_REPRESENTATION(#84,#25165);
#134=CONTEXT_DEPENDENT_SHAPE_REPRESENTATION(#85,#25166);
#135=CONTEXT_DEPENDENT_SHAPE_REPRESENTATION(#86,#25167);
#136=CONTEXT_DEPENDENT_SHAPE_REPRESENTATION(#87,#25168);
#137=CONTEXT_DEPENDENT_SHAPE_REPRESENTATION(#88,#25169);
#138=CONTEXT_DEPENDENT_SHAPE_REPRESENTATION(#89,#25170);
#139=CONTEXT_DEPENDENT_SHAPE_REPRESENTATION(#90,#25171);
#140=CONTEXT_DEPENDENT_SHAPE_REPRESENTATION(#91,#25172);
#141=CONTEXT_DEPENDENT_SHAPE_REPRESENTATION(#92,#25173);
#142=CONTEXT_DEPENDENT_SHAPE_REPRESENTATION(#93,#25174);
#143=CONTEXT_DEPENDENT_SHAPE_REPRESENTATION(#94,#25175);
#144=CONTEXT_DEPENDENT_SHAPE_REPRESENTATION(#95,#25176);
#145=CONTEXT_DEPENDENT_SHAPE_REPRESENTATION(#96,#25177);
#146=CONTEXT_DEPENDENT_SHAPE_REPRESENTATION(#97,#25178);
#147=CONTEXT_DEPENDENT_SHAPE_REPRESENTATION(#98,#25179);
#148=CONTEXT_DEPENDENT_SHAPE_REPRESENTATION(#99,#25180);
#149=CONTEXT_DEPENDENT_SHAPE_REPRESENTATION(#100,#25181);
#150=CONTEXT_DEPENDENT_SHAPE_REPRESENTATION(#101,#25182);
#151=CONTEXT_DEPENDENT_SHAPE_REPRESENTATION(#102,#25183);
#152=CONTEXT_DEPENDENT_SHAPE_REPRESENTATION(#103,#25184);
#153=CONTEXT_DEPENDENT_SHAPE_REPRESENTATION(#104,#25185);
#154=CONTEXT_DEPENDENT_SHAPE_REPRESENTATION(#105,#25186);
#155=CONTEXT_DEPENDENT_SHAPE_REPRESENTATION(#106,#25187);
#156=CONTEXT_DEPENDENT_SHAPE_REPRESENTATION(#107,#25188);
#157=CONTEXT_DEPENDENT_SHAPE_REPRESENTATION(#108,#25189);
#158=CONTEXT_DEPENDENT_SHAPE_REPRESENTATION(#109,#25190);
#159=CONTEXT_DEPENDENT_SHAPE_REPRESENTATION(#110,#25191);
#160=CONTEXT_DEPENDENT_SHAPE_REPRESENTATION(#111,#25192);
#161=CONTEXT_DEPENDENT_SHAPE_REPRESENTATION(#112,#25193);
#162=NEXT_ASSEMBLY_USAGE_OCCURRENCE('Inner ring:1','Inner ring:1',
'Inner ring:1',#25237,#25238,'Inner ring:1');
#163=NEXT_ASSEMBLY_USAGE_OCCURRENCE('Outer ring:1','Outer ring:1',
'Outer ring:1',#25237,#25239,'Outer ring:1');
#164=NEXT_ASSEMBLY_USAGE_OCCURRENCE('Balls:1','Balls:1','Balls:1',#25237,
#25240,'Balls:1');
#165=NEXT_ASSEMBLY_USAGE_OCCURRENCE('Cage:1','Cage:1','Cage:1',#25237,#25241,
'Cage:1');
#166=NEXT_ASSEMBLY_USAGE_OCCURRENCE('Seals 2RS:1','Seals 2RS:1',
'Seals 2RS:1',#25237,#25242,'Seals 2RS:1');
#167=NEXT_ASSEMBLY_USAGE_OCCURRENCE('Moving jaw:1','Moving jaw:1',
'Moving jaw:1',#25243,#25244,'Moving jaw:1');
#168=NEXT_ASSEMBLY_USAGE_OCCURRENCE('Gib:1','Gib:1','Gib:1',#25243,#25245,
'Gib:1');
#169=NEXT_ASSEMBLY_USAGE_OCCURRENCE(
'Seventy-five millimetre jaw insert (1):1',
'Seventy-five millimetre jaw insert (1):1',
'Seventy-five millimetre jaw insert (1):1',#25243,#25246,
'Seventy-five millimetre jaw insert (1):1');
#170=NEXT_ASSEMBLY_USAGE_OCCURRENCE('Flanged lead nut:1',
'Flanged lead nut:1','Flanged lead nut:1',#25243,#25247,
'Flanged lead nut:1');
#171=NEXT_ASSEMBLY_USAGE_OCCURRENCE('Cap Screw - M5x20:2',
'Cap Screw - M5x20:2','Cap Screw - M5x20:2',#25243,#25248,
'Cap Screw - M5x20:2');
#172=NEXT_ASSEMBLY_USAGE_OCCURRENCE('Cap Screw - M5x20:3',
'Cap Screw - M5x20:3','Cap Screw - M5x20:3',#25243,#25248,
'Cap Screw - M5x20:3');
#173=NEXT_ASSEMBLY_USAGE_OCCURRENCE('Cap Screw - M5x20:6',
'Cap Screw - M5x20:6','Cap Screw - M5x20:6',#25243,#25248,
'Cap Screw - M5x20:6');
#174=NEXT_ASSEMBLY_USAGE_OCCURRENCE('Cap Screw - M5x20:7',
'Cap Screw - M5x20:7','Cap Screw - M5x20:7',#25243,#25248,
'Cap Screw - M5x20:7');
#175=NEXT_ASSEMBLY_USAGE_OCCURRENCE('Cap Screw - M4x16:5',
'Cap Screw - M4x16:5','Cap Screw - M4x16:5',#25243,#25249,
'Cap Screw - M4x16:5');
#176=NEXT_ASSEMBLY_USAGE_OCCURRENCE('Cap Screw - M4x16:6',
'Cap Screw - M4x16:6','Cap Screw - M4x16:6',#25243,#25249,
'Cap Screw - M4x16:6');
#177=NEXT_ASSEMBLY_USAGE_OCCURRENCE('Cap Screw - M4x16:7',
'Cap Screw - M4x16:7','Cap Screw - M4x16:7',#25243,#25249,
'Cap Screw - M4x16:7');
#178=NEXT_ASSEMBLY_USAGE_OCCURRENCE('Base:1','Base:1','Base:1',#25229,#25230,
'Base:1');
#179=NEXT_ASSEMBLY_USAGE_OCCURRENCE('Dovetail guide:1',
'Dovetail guide:1','Dovetail guide:1',#25229,#25231,'Dovetail guide:1');
#180=NEXT_ASSEMBLY_USAGE_OCCURRENCE('Fixed jaw:1','Fixed jaw:1',
'Fixed jaw:1',#25229,#25232,'Fixed jaw:1');
#181=NEXT_ASSEMBLY_USAGE_OCCURRENCE('Bearing pedestal:1',
'Bearing pedestal:1','Bearing pedestal:1',#25229,#25233,
'Bearing pedestal:1');
#182=NEXT_ASSEMBLY_USAGE_OCCURRENCE('Bearing cap:1','Bearing cap:1',
'Bearing cap:1',#25229,#25234,'Bearing cap:1');
#183=NEXT_ASSEMBLY_USAGE_OCCURRENCE(
'Seventy-five millimetre jaw insert:1',
'Seventy-five millimetre jaw insert:1',
'Seventy-five millimetre jaw insert:1',#25229,#25235,
'Seventy-five millimetre jaw insert:1');
#184=NEXT_ASSEMBLY_USAGE_OCCURRENCE('M6x20 trimmed screw:2',
'M6x20 trimmed screw:2','M6x20 trimmed screw:2',#25229,#25236,
'M6x20 trimmed screw:2');
#185=NEXT_ASSEMBLY_USAGE_OCCURRENCE('M6x20 trimmed screw:3',
'M6x20 trimmed screw:3','M6x20 trimmed screw:3',#25229,#25236,
'M6x20 trimmed screw:3');
#186=NEXT_ASSEMBLY_USAGE_OCCURRENCE('M6x20 trimmed screw:4',
'M6x20 trimmed screw:4','M6x20 trimmed screw:4',#25229,#25236,
'M6x20 trimmed screw:4');
#187=NEXT_ASSEMBLY_USAGE_OCCURRENCE('Cap Screw - M6x25:2',
'Cap Screw - M6x25:2','Cap Screw - M6x25:2',#25229,#25260,
'Cap Screw - M6x25:2');
#188=NEXT_ASSEMBLY_USAGE_OCCURRENCE('Cap Screw - M6x25:3',
'Cap Screw - M6x25:3','Cap Screw - M6x25:3',#25229,#25260,
'Cap Screw - M6x25:3');
#189=NEXT_ASSEMBLY_USAGE_OCCURRENCE('Cap Screw - M6x25:4',
'Cap Screw - M6x25:4','Cap Screw - M6x25:4',#25229,#25260,
'Cap Screw - M6x25:4');
#190=NEXT_ASSEMBLY_USAGE_OCCURRENCE('Cap Screw - M6x25:5',
'Cap Screw - M6x25:5','Cap Screw - M6x25:5',#25229,#25260,
'Cap Screw - M6x25:5');
#191=NEXT_ASSEMBLY_USAGE_OCCURRENCE(
'Sealed Ball Bearing - 20 x 47 x 14 mm:2',
'Sealed Ball Bearing - 20 x 47 x 14 mm:2',
'Sealed Ball Bearing - 20 x 47 x 14 mm:2',#25229,#25237,
'Sealed Ball Bearing - 20 x 47 x 14 mm:2');
#192=NEXT_ASSEMBLY_USAGE_OCCURRENCE('Cap Screw - M4x16:2',
'Cap Screw - M4x16:2','Cap Screw - M4x16:2',#25229,#25249,
'Cap Screw - M4x16:2');
#193=NEXT_ASSEMBLY_USAGE_OCCURRENCE('Cap Screw - M4x16:3',
'Cap Screw - M4x16:3','Cap Screw - M4x16:3',#25229,#25249,
'Cap Screw - M4x16:3');
#194=NEXT_ASSEMBLY_USAGE_OCCURRENCE('Cap Screw - M4x16:4',
'Cap Screw - M4x16:4','Cap Screw - M4x16:4',#25229,#25249,
'Cap Screw - M4x16:4');
#195=NEXT_ASSEMBLY_USAGE_OCCURRENCE('Cap Screw - M5x20:4',
'Cap Screw - M5x20:4','Cap Screw - M5x20:4',#25229,#25248,
'Cap Screw - M5x20:4');
#196=NEXT_ASSEMBLY_USAGE_OCCURRENCE('Cap Screw - M5x20:5',
'Cap Screw - M5x20:5','Cap Screw - M5x20:5',#25229,#25248,
'Cap Screw - M5x20:5');
#197=NEXT_ASSEMBLY_USAGE_OCCURRENCE('Tr12x3 lead screw:1',
'Tr12x3 lead screw:1','Tr12x3 lead screw:1',#25250,#25251,
'Tr12x3 lead screw:1');
#198=NEXT_ASSEMBLY_USAGE_OCCURRENCE('Inner race spacer:1',
'Inner race spacer:1','Inner race spacer:1',#25250,#25252,
'Inner race spacer:1');
#199=NEXT_ASSEMBLY_USAGE_OCCURRENCE('Shaft retaining collar:1',
'Shaft retaining collar:1','Shaft retaining collar:1',#25250,#25253,
'Shaft retaining collar:1');
#200=NEXT_ASSEMBLY_USAGE_OCCURRENCE('Handwheel:1','Handwheel:1',
'Handwheel:1',#25250,#25254,'Handwheel:1');
#201=NEXT_ASSEMBLY_USAGE_OCCURRENCE('Handle pivot sleeve:1',
'Handle pivot sleeve:1','Handle pivot sleeve:1',#25250,#25255,
'Handle pivot sleeve:1');
#202=NEXT_ASSEMBLY_USAGE_OCCURRENCE('Revolving handle:1',
'Revolving handle:1','Revolving handle:1',#25250,#25256,
'Revolving handle:1');
#203=NEXT_ASSEMBLY_USAGE_OCCURRENCE('Socket Set Screw - M5x8:2',
'Socket Set Screw - M5x8:2','Socket Set Screw - M5x8:2',#25250,#25258,
'Socket Set Screw - M5x8:2');
#204=NEXT_ASSEMBLY_USAGE_OCCURRENCE('Key 6x6x20:2','Key 6x6x20:2',
'Key 6x6x20:2',#25250,#25257,'Key 6x6x20:2');
#205=NEXT_ASSEMBLY_USAGE_OCCURRENCE('Socket Set Screw - M5x8:3',
'Socket Set Screw - M5x8:3','Socket Set Screw - M5x8:3',#25250,#25258,
'Socket Set Screw - M5x8:3');
#206=NEXT_ASSEMBLY_USAGE_OCCURRENCE('Flat Washer - M6:2',
'Flat Washer - M6:2','Flat Washer - M6:2',#25250,#25259,
'Flat Washer - M6:2');
#207=NEXT_ASSEMBLY_USAGE_OCCURRENCE('Cap Screw - M6x25:6',
'Cap Screw - M6x25:6','Cap Screw - M6x25:6',#25250,#25260,
'Cap Screw - M6x25:6');
#208=NEXT_ASSEMBLY_USAGE_OCCURRENCE('Fixed frame:1','Fixed frame:1',
'Fixed frame:1',#25228,#25229,'Fixed frame:1');
#209=NEXT_ASSEMBLY_USAGE_OCCURRENCE('Moving jaw Assembly:1',
'Moving jaw Assembly:1','Moving jaw Assembly:1',#25228,#25243,
'Moving jaw Assembly:1');
#210=NEXT_ASSEMBLY_USAGE_OCCURRENCE('Screw and handwheel:1',
'Screw and handwheel:1','Screw and handwheel:1',#25228,#25250,
'Screw and handwheel:1');
#211=B_SPLINE_CURVE_WITH_KNOTS('',3,(#11837,#11838,#11839,#11840,#11841,
#11842,#11843,#11844,#11845,#11846,#11847,#11848,#11849,#11850,#11851,#11852,
#11853,#11854,#11855,#11856,#11857,#11858),.UNSPECIFIED.,.F.,.F.,(4,2,2,
2,2,2,2,2,2,2,4),(0.0789094028588958,0.210573405340968,0.315860108011452,
0.421146810681936,0.522142632548711,0.623138454415485,0.72413427628226,
0.825130098149035,0.930416800819519,1.03570350349,1.16736750597208),
 .UNSPECIFIED.);
#212=B_SPLINE_CURVE_WITH_KNOTS('',3,(#11862,#11863,#11864,#11865,#11866,
#11867,#11868,#11869,#11870,#11871,#11872,#11873,#11874,#11875,#11876,#11877,
#11878,#11879,#11880,#11881,#11882,#11883),.UNSPECIFIED.,.F.,.F.,(4,2,2,
2,2,2,2,2,2,2,4),(0.0774793363974613,0.142088896491891,0.284177792983782,
0.411119756996526,0.514392970548519,0.617666184100513,0.720939397652506,
0.8242126112045,0.951154575217244,1.09324347170913,1.15785303180356),
 .UNSPECIFIED.);
#213=B_SPLINE_CURVE_WITH_KNOTS('',3,(#11889,#11890,#11891,#11892,#11893,
#11894,#11895,#11896,#11897,#11898,#11899,#11900,#11901,#11902,#11903,#11904,
#11905,#11906,#11907,#11908,#11909,#11910),.UNSPECIFIED.,.F.,.F.,(4,2,2,
2,2,2,2,2,2,2,4),(0.0774793363974613,0.142088896491891,0.284177792983782,
0.411119756996525,0.514392970548519,0.617666184100513,0.720939397652506,
0.8242126112045,0.951154575217243,1.09324347170913,1.15785303180356),
 .UNSPECIFIED.);
#214=B_SPLINE_CURVE_WITH_KNOTS('',3,(#11914,#11915,#11916,#11917,#11918,
#11919,#11920,#11921,#11922,#11923,#11924,#11925,#11926,#11927,#11928,#11929,
#11930,#11931,#11932,#11933,#11934,#11935),.UNSPECIFIED.,.F.,.F.,(4,2,2,
2,2,2,2,2,2,2,4),(0.0774793363974614,0.142088896491891,0.284177792983781,
0.411119756996525,0.514392970548519,0.617666184100512,0.720939397652506,
0.824212611204499,0.951154575217243,1.09324347170913,1.15785303180356),
 .UNSPECIFIED.);
#215=B_SPLINE_CURVE_WITH_KNOTS('',3,(#11939,#11940,#11941,#11942,#11943,
#11944,#11945,#11946,#11947,#11948,#11949,#11950),.UNSPECIFIED.,.F.,.F.,
(4,2,2,2,2,4),(0.0774793363974613,0.142088896491891,0.284177792983781,0.411119756996525,
0.514392970548519,0.617666184100512),.UNSPECIFIED.);
#216=B_SPLINE_CURVE_WITH_KNOTS('',3,(#11955,#11956,#11957,#11958,#11959,
#11960,#11961,#11962,#11963,#11964,#11965,#11966),.UNSPECIFIED.,.F.,.F.,
(4,2,2,2,2,4),(0.617666184100512,0.720939397652506,0.824212611204499,0.951154575217243,
1.09324347170913,1.15785303180356),.UNSPECIFIED.);
#217=B_SPLINE_CURVE_WITH_KNOTS('',3,(#11970,#11971,#11972,#11973,#11974,
#11975,#11976,#11977,#11978,#11979,#11980,#11981,#11982,#11983,#11984,#11985,
#11986,#11987,#11988,#11989,#11990,#11991),.UNSPECIFIED.,.F.,.F.,(4,2,2,
2,2,2,2,2,2,2,4),(0.0774793363974613,0.142088896491891,0.284177792983782,
0.411119756996526,0.514392970548519,0.617666184100513,0.720939397652507,
0.8242126112045,0.951154575217245,1.09324347170914,1.15785303180356),
 .UNSPECIFIED.);
#218=B_SPLINE_CURVE_WITH_KNOTS('',3,(#11995,#11996,#11997,#11998,#11999,
#12000,#12001,#12002,#12003,#12004,#12005,#12006,#12007,#12008,#12009,#12010,
#12011,#12012,#12013,#12014,#12015,#12016),.UNSPECIFIED.,.F.,.F.,(4,2,2,
2,2,2,2,2,2,2,4),(0.0774793363974613,0.142088896491891,0.284177792983782,
0.411119756996526,0.514392970548519,0.617666184100513,0.720939397652506,
0.824212611204499,0.951154575217243,1.09324347170913,1.15785303180356),
 .UNSPECIFIED.);
#219=B_SPLINE_CURVE_WITH_KNOTS('',3,(#12020,#12021,#12022,#12023,#12024,
#12025,#12026,#12027,#12028,#12029,#12030,#12031,#12032,#12033,#12034,#12035,
#12036,#12037,#12038,#12039,#12040,#12041),.UNSPECIFIED.,.F.,.F.,(4,2,2,
2,2,2,2,2,2,2,4),(0.0774793363974613,0.142088896491891,0.284177792983782,
0.411119756996526,0.514392970548519,0.617666184100513,0.720939397652506,
0.8242126112045,0.951154575217244,1.09324347170913,1.15785303180356),
 .UNSPECIFIED.);
#220=B_SPLINE_CURVE_WITH_KNOTS('',3,(#12045,#12046,#12047,#12048,#12049,
#12050,#12051,#12052,#12053,#12054,#12055,#12056,#12057,#12058,#12059,#12060,
#12061,#12062,#12063,#12064,#12065,#12066),.UNSPECIFIED.,.F.,.F.,(4,2,2,
2,2,2,2,2,2,2,4),(0.0774793363974613,0.142088896491891,0.284177792983782,
0.411119756996526,0.514392970548519,0.617666184100513,0.720939397652506,
0.8242126112045,0.951154575217243,1.09324347170913,1.15785303180356),
 .UNSPECIFIED.);
#221=B_SPLINE_CURVE_WITH_KNOTS('',3,(#12074,#12075,#12076,#12077,#12078,
#12079,#12080,#12081,#12082,#12083,#12084,#12085,#12086,#12087,#12088,#12089,
#12090,#12091,#12092,#12093,#12094,#12095),.UNSPECIFIED.,.F.,.F.,(4,2,2,
2,2,2,2,2,2,2,4),(0.0789094028588958,0.210573405340968,0.315860108011452,
0.421146810681936,0.522142632548711,0.623138454415485,0.72413427628226,
0.825130098149035,0.930416800819519,1.03570350349,1.16736750597208),
 .UNSPECIFIED.);
#222=B_SPLINE_CURVE_WITH_KNOTS('',3,(#12103,#12104,#12105,#12106,#12107,
#12108,#12109,#12110,#12111,#12112,#12113,#12114,#12115,#12116,#12117,#12118,
#12119,#12120,#12121,#12122,#12123,#12124),.UNSPECIFIED.,.F.,.F.,(4,2,2,
2,2,2,2,2,2,2,4),(0.0789094028588958,0.210573405340969,0.315860108011453,
0.421146810681937,0.522142632548712,0.623138454415486,0.724134276282261,
0.825130098149035,0.930416800819519,1.03570350349,1.16736750597208),
 .UNSPECIFIED.);
#223=B_SPLINE_CURVE_WITH_KNOTS('',3,(#12133,#12134,#12135,#12136,#12137,
#12138,#12139,#12140,#12141,#12142,#12143,#12144),.UNSPECIFIED.,.F.,.F.,
(4,2,2,2,2,4),(0.0789094028588958,0.210573405340968,0.315860108011452,0.421146810681937,
0.522142632548711,0.623138454415486),.UNSPECIFIED.);
#224=B_SPLINE_CURVE_WITH_KNOTS('',3,(#12146,#12147,#12148,#12149,#12150,
#12151,#12152,#12153,#12154,#12155,#12156,#12157),.UNSPECIFIED.,.F.,.F.,
(4,2,2,2,2,4),(0.623138454415486,0.72413427628226,0.825130098149035,0.930416800819519,
1.03570350349,1.16736750597208),.UNSPECIFIED.);
#225=B_SPLINE_CURVE_WITH_KNOTS('',3,(#12164,#12165,#12166,#12167,#12168,
#12169,#12170,#12171,#12172,#12173,#12174,#12175,#12176,#12177,#12178,#12179,
#12180,#12181,#12182,#12183,#12184,#12185),.UNSPECIFIED.,.F.,.F.,(4,2,2,
2,2,2,2,2,2,2,4),(0.0789094028588958,0.210573405340968,0.315860108011452,
0.421146810681936,0.522142632548711,0.623138454415486,0.72413427628226,
0.825130098149035,0.930416800819519,1.03570350349,1.16736750597208),
 .UNSPECIFIED.);
#226=B_SPLINE_CURVE_WITH_KNOTS('',3,(#12193,#12194,#12195,#12196,#12197,
#12198,#12199,#12200,#12201,#12202,#12203,#12204,#12205,#12206,#12207,#12208,
#12209,#12210,#12211,#12212,#12213,#12214),.UNSPECIFIED.,.F.,.F.,(4,2,2,
2,2,2,2,2,2,2,4),(0.0789094028588957,0.210573405340968,0.315860108011452,
0.421146810681936,0.522142632548711,0.623138454415485,0.72413427628226,
0.825130098149035,0.930416800819519,1.03570350349,1.16736750597207),
 .UNSPECIFIED.);
#227=B_SPLINE_CURVE_WITH_KNOTS('',3,(#12222,#12223,#12224,#12225,#12226,
#12227,#12228,#12229,#12230,#12231,#12232,#12233,#12234,#12235,#12236,#12237,
#12238,#12239,#12240,#12241,#12242,#12243),.UNSPECIFIED.,.F.,.F.,(4,2,2,
2,2,2,2,2,2,2,4),(0.0789094028588958,0.210573405340968,0.315860108011452,
0.421146810681936,0.522142632548711,0.623138454415486,0.72413427628226,
0.825130098149035,0.930416800819519,1.03570350349,1.16736750597208),
 .UNSPECIFIED.);
#228=B_SPLINE_CURVE_WITH_KNOTS('',3,(#12252,#12253,#12254,#12255,#12256,
#12257,#12258,#12259,#12260,#12261,#12262,#12263,#12264,#12265,#12266,#12267,
#12268,#12269,#12270,#12271,#12272,#12273),.UNSPECIFIED.,.F.,.F.,(4,2,2,
2,2,2,2,2,2,2,4),(0.0789094028588958,0.210573405340968,0.315860108011452,
0.421146810681936,0.522142632548711,0.623138454415485,0.72413427628226,
0.825130098149035,0.930416800819519,1.03570350349,1.16736750597208),
 .UNSPECIFIED.);
#229=B_SPLINE_CURVE_WITH_KNOTS('',3,(#12520,#12521,#12522,#12523,#12524,
#12525,#12526,#12527,#12528,#12529,#12530,#12531,#12532,#12533,#12534,#12535,
#12536,#12537,#12538,#12539,#12540,#12541,#12542,#12543,#12544),
 .UNSPECIFIED.,.F.,.F.,(4,3,3,3,3,3,3,3,4),(-3.56038179279204,-3.46201024481372,
-2.96743735269747,-2.47286446058123,-1.97829156846498,-1.48371867634874,
-0.989145784232491,-0.494572892116246,0.),.UNSPECIFIED.);
#230=B_SPLINE_CURVE_WITH_KNOTS('',3,(#12547,#12548,#12549,#12550,#12551,
#12552,#12553,#12554,#12555,#12556,#12557,#12558,#12559,#12560,#12561,#12562,
#12563,#12564,#12565,#12566,#12567,#12568,#12569,#12570,#12571,#12572,#12573,
#12574,#12575,#12576,#12577,#12578,#12579,#12580,#12581,#12582,#12583,#12584,
#12585,#12586),.UNSPECIFIED.,.F.,.F.,(4,3,3,3,3,3,3,3,3,3,3,3,3,4),(0.937891254796418,
0.989145784232494,1.48371867634874,1.97829156846498,2.47286446058123,2.96743735269748,
3.46201024481372,3.95658313692997,4.45115602904621,4.94572892116246,5.44030181327871,
5.93487470539495,6.42944759751119,6.80228742277363),.UNSPECIFIED.);
#231=B_SPLINE_CURVE_WITH_KNOTS('',3,(#12591,#12592,#12593,#12594,#12595,
#12596,#12597,#12598,#12599,#12600,#12601,#12602,#12603,#12604,#12605,#12606,
#12607,#12608,#12609,#12610,#12611,#12612,#12613,#12614,#12615,#12616,#12617,
#12618,#12619,#12620,#12621,#12622,#12623,#12624,#12625,#12626,#12627,#12628,
#12629,#12630),.UNSPECIFIED.,.F.,.F.,(4,3,3,3,3,3,3,3,3,3,3,3,3,4),(-9.8435670999716,
-9.39688495020867,-8.90231205809242,-8.40773916597618,-7.91316627385993,
-7.41859338174369,-6.92402048962744,-6.42944759751119,-5.93487470539495,
-5.4403018132787,-4.94572892116246,-4.45115602904621,-3.95658313692996,
-3.56038179279204),.UNSPECIFIED.);
#232=B_SPLINE_CURVE_WITH_KNOTS('',3,(#12631,#12632,#12633,#12634,#12635,
#12636,#12637,#12638,#12639,#12640,#12641,#12642,#12643,#12644,#12645,#12646,
#12647,#12648,#12649,#12650,#12651,#12652,#12653,#12654,#12655,#12656,#12657,
#12658,#12659,#12660,#12661,#12662,#12663,#12664,#12665,#12666,#12667,#12668,
#12669,#12670,#12671,#12672,#12673),.UNSPECIFIED.,.F.,.F.,(4,3,3,3,3,3,
3,3,3,3,3,3,3,3,4),(6.80228742277363,6.92402048962744,7.41859338174369,
7.91316627385993,8.40773916597617,8.90231205809242,9.39688495020867,9.89145784232491,
10.3860307344412,10.8806036265574,11.3751765186736,11.8697494107899,12.3643223029061,
12.8588951950224,13.0854727299532),.UNSPECIFIED.);
#233=B_SPLINE_CURVE_WITH_KNOTS('',3,(#12678,#12679,#12680,#12681,#12682,
#12683,#12684,#12685,#12686,#12687,#12688,#12689,#12690,#12691,#12692,#12693,
#12694,#12695,#12696,#12697,#12698,#12699,#12700,#12701,#12702,#12703,#12704,
#12705,#12706,#12707,#12708,#12709,#12710,#12711,#12712,#12713,#12714,#12715,
#12716,#12717,#12718,#12719,#12720),.UNSPECIFIED.,.F.,.F.,(4,3,3,3,3,3,
3,3,3,3,3,3,3,3,4),(-16.1267524071512,-15.8263325477199,-15.3317596556036,
-14.8371867634874,-14.3426138713711,-13.8480409792549,-13.3534680871386,
-12.8588951950224,-12.3643223029061,-11.8697494107899,-11.3751765186736,
-10.8806036265574,-10.3860307344412,-9.89145784232491,-9.8435670999716),
 .UNSPECIFIED.);
#234=B_SPLINE_CURVE_WITH_KNOTS('',3,(#12721,#12722,#12723,#12724,#12725,
#12726,#12727,#12728,#12729,#12730,#12731,#12732,#12733,#12734,#12735,#12736,
#12737,#12738,#12739,#12740,#12741,#12742,#12743,#12744,#12745,#12746,#12747,
#12748,#12749,#12750,#12751,#12752,#12753,#12754,#12755,#12756,#12757,#12758,
#12759,#12760,#12761,#12762,#12763),.UNSPECIFIED.,.F.,.F.,(4,3,3,3,3,3,
3,3,3,3,3,3,3,3,4),(13.0854727299532,13.3534680871386,13.8480409792549,
14.3426138713711,14.8371867634874,15.3317596556036,15.8263325477199,16.3209054398361,
16.8154783319523,17.3100512240686,17.8046241161848,18.2991970083011,18.7937699004173,
19.2883427925336,19.3686580371328),.UNSPECIFIED.);
#235=B_SPLINE_CURVE_WITH_KNOTS('',3,(#12768,#12769,#12770,#12771,#12772,
#12773,#12774,#12775,#12776,#12777,#12778,#12779,#12780,#12781,#12782,#12783,
#12784,#12785,#12786,#12787,#12788,#12789,#12790,#12791,#12792,#12793,#12794,
#12795,#12796,#12797,#12798,#12799,#12800,#12801,#12802,#12803,#12804,#12805,
#12806,#12807,#12808,#12809,#12810),.UNSPECIFIED.,.F.,.F.,(4,3,3,3,3,3,
3,3,3,3,3,3,3,3,4),(-22.4099377143308,-22.2557801452311,-21.7612072531148,
-21.2666343609986,-20.7720614688823,-20.2774885767661,-19.7829156846498,
-19.2883427925336,-18.7937699004173,-18.2991970083011,-17.8046241161848,
-17.3100512240686,-16.8154783319523,-16.3209054398361,-16.1267524071512),
 .UNSPECIFIED.);
#236=B_SPLINE_CURVE_WITH_KNOTS('',3,(#12811,#12812,#12813,#12814,#12815,
#12816,#12817,#12818,#12819,#12820,#12821,#12822,#12823,#12824,#12825,#12826,
#12827,#12828,#12829,#12830,#12831,#12832,#12833,#12834,#12835,#12836,#12837,
#12838,#12839,#12840,#12841,#12842,#12843,#12844,#12845,#12846,#12847,#12848,
#12849,#12850),.UNSPECIFIED.,.F.,.F.,(4,3,3,3,3,3,3,3,3,3,3,3,3,4),(19.3686580371328,
19.7829156846498,20.2774885767661,20.7720614688823,21.2666343609986,21.7612072531148,
22.255780145231,22.7503530373473,23.2449259294635,23.7394988215798,24.234071713696,
24.7286446058123,25.2232174979285,25.6518433443124),.UNSPECIFIED.);
#237=B_SPLINE_CURVE_WITH_KNOTS('',3,(#12855,#12856,#12857,#12858,#12859,
#12860,#12861,#12862,#12863,#12864,#12865,#12866,#12867,#12868,#12869,#12870,
#12871,#12872,#12873,#12874,#12875,#12876,#12877,#12878,#12879,#12880,#12881,
#12882,#12883,#12884,#12885,#12886,#12887,#12888,#12889,#12890,#12891,#12892,
#12893,#12894,#12895,#12896,#12897),.UNSPECIFIED.,.F.,.F.,(4,3,3,3,3,3,
3,3,3,3,3,3,3,3,4),(-28.6931230215104,-28.6852277427422,-28.190654850626,
-27.6960819585097,-27.2015090663935,-26.7069361742773,-26.212363282161,
-25.7177903900448,-25.2232174979285,-24.7286446058123,-24.234071713696,
-23.7394988215798,-23.2449259294635,-22.7503530373473,-22.4099377143308),
 .UNSPECIFIED.);
#238=B_SPLINE_CURVE_WITH_KNOTS('',3,(#12898,#12899,#12900,#12901,#12902,
#12903,#12904,#12905,#12906,#12907,#12908,#12909,#12910,#12911,#12912,#12913,
#12914,#12915,#12916,#12917,#12918,#12919,#12920,#12921,#12922,#12923,#12924,
#12925,#12926,#12927,#12928,#12929,#12930,#12931,#12932,#12933,#12934,#12935,
#12936,#12937,#12938,#12939,#12940),.UNSPECIFIED.,.F.,.F.,(4,3,3,3,3,3,
3,3,3,3,3,3,3,3,4),(25.6518433443124,25.7177903900448,26.212363282161,26.7069361742773,
27.2015090663935,27.6960819585097,28.190654850626,28.6852277427422,29.1798006348585,
29.6743735269747,30.168946419091,30.6635193112072,31.1580922033235,31.6526650954397,
31.935028651492),.UNSPECIFIED.);
#239=B_SPLINE_CURVE_WITH_KNOTS('',3,(#12945,#12946,#12947,#12948,#12949,
#12950,#12951,#12952,#12953,#12954,#12955,#12956,#12957,#12958,#12959,#12960,
#12961,#12962,#12963,#12964,#12965,#12966,#12967,#12968,#12969,#12970,#12971,
#12972,#12973,#12974,#12975,#12976,#12977,#12978,#12979,#12980,#12981,#12982,
#12983,#12984),.UNSPECIFIED.,.F.,.F.,(4,3,3,3,3,3,3,3,3,3,3,3,3,4),(-34.97630832869,
-34.6201024481372,-34.1255295560209,-33.6309566639047,-33.1363837717884,
-32.6418108796722,-32.147237987556,-31.6526650954397,-31.1580922033235,
-30.6635193112072,-30.168946419091,-29.6743735269747,-29.1798006348585,
-28.6931230215104),.UNSPECIFIED.);
#240=B_SPLINE_CURVE_WITH_KNOTS('',3,(#12985,#12986,#12987,#12988,#12989,
#12990,#12991,#12992,#12993,#12994,#12995,#12996,#12997,#12998,#12999,#13000,
#13001,#13002,#13003,#13004,#13005,#13006,#13007,#13008,#13009,#13010,#13011,
#13012,#13013,#13014,#13015,#13016,#13017,#13018,#13019,#13020,#13021,#13022,
#13023,#13024,#13025,#13026,#13027),.UNSPECIFIED.,.F.,.F.,(4,3,3,3,3,3,
3,3,3,3,3,3,3,3,4),(31.935028651492,32.147237987556,32.6418108796722,33.1363837717885,
33.6309566639047,34.1255295560209,34.6201024481372,35.1146753402534,35.6092482323697,
36.1038211244859,36.5983940166022,37.0929669087184,37.5875398008347,38.0821126929509,
38.2182139586716),.UNSPECIFIED.);
#241=B_SPLINE_CURVE_WITH_KNOTS('',3,(#13032,#13033,#13034,#13035,#13036,
#13037,#13038,#13039,#13040,#13041,#13042,#13043,#13044,#13045,#13046,#13047,
#13048,#13049,#13050,#13051,#13052,#13053,#13054,#13055,#13056,#13057,#13058,
#13059,#13060,#13061,#13062,#13063,#13064,#13065,#13066,#13067,#13068,#13069,
#13070,#13071,#13072,#13073,#13074),.UNSPECIFIED.,.F.,.F.,(4,3,3,3,3,3,
3,3,3,3,3,3,3,3,4),(-41.2594936358696,-41.0495500456484,-40.5549771535321,
-40.0604042614159,-39.5658313692996,-39.0712584771834,-38.5766855850671,
-38.0821126929509,-37.5875398008347,-37.0929669087184,-36.5983940166022,
-36.1038211244859,-35.6092482323697,-35.1146753402534,-34.97630832869),
 .UNSPECIFIED.);
#242=B_SPLINE_CURVE_WITH_KNOTS('',3,(#13075,#13076,#13077,#13078,#13079,
#13080,#13081,#13082,#13083,#13084,#13085,#13086,#13087,#13088,#13089,#13090,
#13091,#13092,#13093,#13094,#13095,#13096,#13097,#13098,#13099,#13100,#13101,
#13102,#13103,#13104,#13105,#13106,#13107,#13108,#13109,#13110,#13111,#13112,
#13113,#13114),.UNSPECIFIED.,.F.,.F.,(4,3,3,3,3,3,3,3,3,3,3,3,3,4),(38.2182139586716,
38.5766855850671,39.0712584771834,39.5658313692996,40.0604042614159,40.5549771535321,
41.0495500456484,41.5441229377646,42.0386958298809,42.5332687219971,43.0278416141134,
43.5224145062296,44.0169873983459,44.5013992658512),.UNSPECIFIED.);
#243=B_SPLINE_CURVE_WITH_KNOTS('',3,(#13119,#13120,#13121,#13122,#13123,
#13124,#13125,#13126,#13127,#13128,#13129,#13130,#13131,#13132,#13133,#13134,
#13135,#13136,#13137,#13138,#13139,#13140,#13141,#13142,#13143,#13144,#13145,
#13146,#13147,#13148,#13149,#13150,#13151,#13152,#13153,#13154,#13155,#13156,
#13157,#13158,#13159,#13160,#13161),.UNSPECIFIED.,.F.,.F.,(4,3,3,3,3,3,
3,3,3,3,3,3,3,3,4),(-47.5426789430491,-47.4789976431596,-46.9844247510433,
-46.4898518589271,-45.9952789668108,-45.5007060746946,-45.0061331825783,
-44.5115602904621,-44.0169873983458,-43.5224145062296,-43.0278416141134,
-42.5332687219971,-42.0386958298809,-41.5441229377646,-41.2594936358696),
 .UNSPECIFIED.);
#244=B_SPLINE_CURVE_WITH_KNOTS('',3,(#13162,#13163,#13164,#13165,#13166,
#13167,#13168,#13169,#13170,#13171,#13172,#13173,#13174,#13175,#13176,#13177,
#13178,#13179,#13180,#13181,#13182,#13183,#13184,#13185,#13186,#13187,#13188,
#13189,#13190,#13191,#13192,#13193,#13194,#13195,#13196,#13197,#13198,#13199,
#13200,#13201,#13202,#13203,#13204),.UNSPECIFIED.,.F.,.F.,(4,3,3,3,3,3,
3,3,3,3,3,3,3,3,4),(44.5013992658512,44.5115602904621,45.0061331825783,
45.5007060746946,45.9952789668108,46.4898518589271,46.9844247510433,47.4789976431596,
47.9735705352758,48.4681434273921,48.9627163195083,49.4572892116245,49.9518621037408,
50.446434995857,50.7845845730308),.UNSPECIFIED.);
#245=B_SPLINE_CURVE_WITH_KNOTS('',3,(#13211,#13212,#13213,#13214,#13215,
#13216,#13217,#13218,#13219,#13220),.UNSPECIFIED.,.F.,.F.,(4,3,3,4),(-54.4542726622231,
-54.403018132787,-53.9084452406708,-53.8258642502287),.UNSPECIFIED.);
#246=B_SPLINE_CURVE_WITH_KNOTS('',3,(#13226,#13227,#13228,#13229,#13230,
#13231,#13232),.UNSPECIFIED.,.F.,.F.,(4,1,1,1,4),(65.9734457253856,66.0560267158277,
66.5505996079439,67.0451725000601,67.5397453921764),.UNSPECIFIED.);
#247=B_SPLINE_CURVE_WITH_KNOTS('',3,(#13235,#13236,#13237,#13238,#13239,
#13240,#13241,#13242,#13243,#13244,#13245,#13246),.UNSPECIFIED.,.F.,.F.,
(4,1,1,1,1,1,1,1,1,4),(65.9734457253856,66.1298690403281,66.6244419324444,
67.1190148245607,67.6135877166769,68.1081606087931,68.6027335009094,69.0973063930256,
69.5918792851419,69.643133814578),.UNSPECIFIED.);
#248=B_SPLINE_CURVE_WITH_KNOTS('',3,(#13251,#13252,#13253,#13254,#13255,
#13256,#13257,#13258,#13259,#13260,#13261,#13262,#13263,#13264,#13265,#13266),
 .UNSPECIFIED.,.F.,.F.,(4,1,1,1,1,1,1,1,1,1,1,1,1,4),(59.6902604182061,
60.1211520104327,60.615724902549,61.1102977946652,61.6048706867815,62.0994435788977,
62.5940164710139,63.0885893631302,63.5831622552464,64.0777351473627,64.5723080394789,
65.0668809315952,65.5614538237114,65.9734457253856),.UNSPECIFIED.);
#249=B_SPLINE_CURVE_WITH_KNOTS('',3,(#13267,#13268,#13269,#13270,#13271,
#13272,#13273,#13274,#13275,#13276,#13277,#13278,#13279,#13280,#13281,#13282,
#13283),.UNSPECIFIED.,.F.,.F.,(4,1,1,1,1,1,1,1,1,1,1,1,1,1,4),(59.6902604182061,
59.700421442817,60.1949943349332,60.6895672270495,61.1841401191657,61.6787130112819,
62.1732859033982,62.6678587955144,63.1624316876307,63.6570045797469,64.1515774718632,
64.6461503639794,65.1407232560957,65.6352961482119,65.9734457253856),
 .UNSPECIFIED.);
#250=B_SPLINE_CURVE_WITH_KNOTS('',3,(#13288,#13289,#13290,#13291,#13292,
#13293,#13294,#13295,#13296,#13297,#13298,#13299,#13300,#13301,#13302,#13303,
#13304),.UNSPECIFIED.,.F.,.F.,(4,1,1,1,1,1,1,1,1,1,1,1,1,1,4),(53.4070751110264,
53.6917044129215,54.1862773050378,54.680850197154,55.1754230892703,55.6699959813865,
56.1645688735028,56.659141765619,57.1537146577353,57.6482875498515,58.1428604419677,
58.637433334084,59.1320062262002,59.6265791183165,59.6902604182061),
 .UNSPECIFIED.);
#251=B_SPLINE_CURVE_WITH_KNOTS('',3,(#13305,#13306,#13307,#13308,#13309,
#13310,#13311,#13312,#13313,#13314,#13315,#13316,#13317,#13318,#13319,#13320),
 .UNSPECIFIED.,.F.,.F.,(4,1,1,1,1,1,1,1,1,1,1,1,1,4),(53.4070751110264,
53.765546737422,54.2601196295383,54.7546925216545,55.2492654137708,55.743838305887,
56.2384111980032,56.7329840901195,57.2275569822357,57.722129874352,58.2167027664682,
58.7112756585845,59.2058485507007,59.6902604182061),.UNSPECIFIED.);
#252=B_SPLINE_CURVE_WITH_KNOTS('',3,(#13325,#13326,#13327,#13328,#13329,
#13330,#13331,#13332,#13333,#13334,#13335,#13336,#13337,#13338,#13339,#13340,
#13341),.UNSPECIFIED.,.F.,.F.,(4,1,1,1,1,1,1,1,1,1,1,1,1,1,4),(47.1238898038469,
47.2622568154103,47.7568297075266,48.2514025996428,48.7459754917591,49.2405483838753,
49.7351212759916,50.2296941681078,50.7242670602241,51.2188399523403,51.7134128444565,
52.2079857365728,52.702558628689,53.1971315208053,53.4070751110264),
 .UNSPECIFIED.);
#253=B_SPLINE_CURVE_WITH_KNOTS('',3,(#13342,#13343,#13344,#13345,#13346,
#13347,#13348,#13349,#13350,#13351,#13352,#13353,#13354,#13355,#13356,#13357,
#13358),.UNSPECIFIED.,.F.,.F.,(4,1,1,1,1,1,1,1,1,1,1,1,1,1,4),(47.1238898038469,
47.3360991399108,47.8306720320271,48.3252449241433,48.8198178162596,49.3143907083758,
49.8089636004921,50.3035364926083,50.7981093847245,51.2926822768408,51.787255168957,
52.2818280610733,52.7764009531895,53.2709738453058,53.4070751110264),
 .UNSPECIFIED.);
#254=B_SPLINE_CURVE_WITH_KNOTS('',3,(#13363,#13364,#13365,#13366,#13367,
#13368,#13369,#13370,#13371,#13372,#13373,#13374,#13375,#13376,#13377,#13378),
 .UNSPECIFIED.,.F.,.F.,(4,1,1,1,1,1,1,1,1,1,1,1,1,4),(40.8407044966673,
41.3273821100154,41.8219550021316,42.3165278942479,42.8111007863641,43.3056736784804,
43.8002465705966,44.2948194627129,44.7893923548291,45.2839652469454,45.7785381390616,
46.2731110311778,46.7676839232941,47.1238898038469),.UNSPECIFIED.);
#255=B_SPLINE_CURVE_WITH_KNOTS('',3,(#13379,#13380,#13381,#13382,#13383,
#13384,#13385,#13386,#13387,#13388,#13389,#13390,#13391,#13392,#13393,#13394,
#13395),.UNSPECIFIED.,.F.,.F.,(4,1,1,1,1,1,1,1,1,1,1,1,1,1,4),(40.8407044966673,
40.9066515423996,41.4012244345159,41.8957973266321,42.3903702187484,42.8849431108646,
43.3795160029809,43.8740888950971,44.3686617872134,44.8632346793296,45.3578075714458,
45.8523804635621,46.3469533556783,46.8415262477946,47.1238898038469),
 .UNSPECIFIED.);
#256=B_SPLINE_CURVE_WITH_KNOTS('',3,(#13400,#13401,#13402,#13403,#13404,
#13405,#13406,#13407,#13408,#13409,#13410,#13411,#13412,#13413,#13414,#13415,
#13416),.UNSPECIFIED.,.F.,.F.,(4,1,1,1,1,1,1,1,1,1,1,1,1,1,4),(34.5575191894877,
34.8979345125042,35.3925074046204,35.8870802967367,36.3816531888529,36.8762260809692,
37.3707989730854,37.8653718652017,38.3599447573179,38.8545176494342,39.3490905415504,
39.8436634336667,40.3382363257829,40.8328092178991,40.8407044966673),
 .UNSPECIFIED.);
#257=B_SPLINE_CURVE_WITH_KNOTS('',3,(#13417,#13418,#13419,#13420,#13421,
#13422,#13423,#13424,#13425,#13426,#13427,#13428,#13429,#13430,#13431,#13432),
 .UNSPECIFIED.,.F.,.F.,(4,1,1,1,1,1,1,1,1,1,1,1,1,4),(34.5575191894877,
34.9717768370047,35.4663497291209,35.9609226212372,36.4554955133534,36.9500684054697,
37.4446412975859,37.9392141897022,38.4337870818184,38.9283599739347,39.4229328660509,
39.9175057581671,40.4120786502834,40.8407044966673),.UNSPECIFIED.);
#258=B_SPLINE_CURVE_WITH_KNOTS('',3,(#13437,#13438,#13439,#13440,#13441,
#13442,#13443,#13444,#13445,#13446,#13447,#13448,#13449,#13450,#13451,#13452,
#13453),.UNSPECIFIED.,.F.,.F.,(4,1,1,1,1,1,1,1,1,1,1,1,1,1,4),(28.2743338823081,
28.468486914993,28.9630598071093,29.4576326992255,29.9522055913417,30.446778483458,
30.9413513755742,31.4359242676905,31.9304971598067,32.425070051923,32.9196429440392,
33.4142158361555,33.9087887282717,34.403361620388,34.5575191894877),
 .UNSPECIFIED.);
#259=B_SPLINE_CURVE_WITH_KNOTS('',3,(#13454,#13455,#13456,#13457,#13458,
#13459,#13460,#13461,#13462,#13463,#13464,#13465,#13466,#13467,#13468,#13469,
#13470),.UNSPECIFIED.,.F.,.F.,(4,1,1,1,1,1,1,1,1,1,1,1,1,1,4),(28.2743338823081,
28.5423292394935,29.0369021316097,29.531475023726,30.0260479158422,30.5206208079585,
31.0151937000747,31.509766592191,32.0043394843072,32.4989123764235,32.9934852685397,
33.488058160656,33.9826310527722,34.4772039448884,34.5575191894877),
 .UNSPECIFIED.);
#260=B_SPLINE_CURVE_WITH_KNOTS('',3,(#13475,#13476,#13477,#13478,#13479,
#13480,#13481,#13482,#13483,#13484,#13485,#13486,#13487,#13488,#13489,#13490,
#13491),.UNSPECIFIED.,.F.,.F.,(4,1,1,1,1,1,1,1,1,1,1,1,1,1,4),(21.9911485751285,
22.0390393174818,22.5336122095981,23.0281851017143,23.5227579938306,24.0173308859468,
24.511903778063,25.0064766701793,25.5010495622955,25.9956224544118,26.490195346528,
26.9847682386443,27.4793411307605,27.9739140228768,28.2743338823081),
 .UNSPECIFIED.);
#261=B_SPLINE_CURVE_WITH_KNOTS('',3,(#13492,#13493,#13494,#13495,#13496,
#13497,#13498,#13499,#13500,#13501,#13502,#13503,#13504,#13505,#13506,#13507,
#13508),.UNSPECIFIED.,.F.,.F.,(4,1,1,1,1,1,1,1,1,1,1,1,1,1,4),(21.9911485751285,
22.1128816419823,22.6074545340986,23.1020274262148,23.596600318331,24.0911732104473,
24.5857461025635,25.0803189946798,25.574891886796,26.0694647789123,26.5640376710285,
27.0586105631448,27.553183455261,28.0477563473773,28.2743338823081),
 .UNSPECIFIED.);
#262=B_SPLINE_CURVE_WITH_KNOTS('',3,(#13514,#13515,#13516,#13517,#13518),
 .UNSPECIFIED.,.F.,.F.,(4,1,4),(15.1888611523549,15.6834340444711,15.7079632679489),
 .UNSPECIFIED.);
#263=B_SPLINE_CURVE_WITH_KNOTS('',3,(#13521,#13522,#13523,#13524,#13525,
#13526,#13527,#13528,#13529,#13530),.UNSPECIFIED.,.F.,.F.,(4,1,1,1,1,1,
1,4),(13.0854727299533,13.1367272593894,13.6313001515056,14.1258730436219,
14.6204459357381,15.1150188278544,15.6095917199706,15.7079632679489),
 .UNSPECIFIED.);
#264=B_SPLINE_CURVE_WITH_KNOTS('',3,(#13532,#13533,#13534,#13535,#13536,
#13537,#13538,#13539,#13540,#13541,#13542,#13543,#13544,#13545,#13546,#13547),
 .UNSPECIFIED.,.F.,.F.,(4,1,1,1,1,1,1,1,1,1,1,1,1,4),(15.7079632679489,
16.1041646120869,16.5987375042031,17.0933103963194,17.5878832884356,18.0824561805519,
18.5770290726681,19.0716019647843,19.5661748569006,20.0607477490168,20.5553206411331,
21.0498935332493,21.5444664253656,21.9911485751285),.UNSPECIFIED.);
#265=B_SPLINE_CURVE_WITH_KNOTS('',3,(#13548,#13549,#13550,#13551,#13552,
#13553,#13554,#13555,#13556,#13557,#13558,#13559,#13560,#13561,#13562,#13563),
 .UNSPECIFIED.,.F.,.F.,(4,1,1,1,1,1,1,1,1,1,1,1,1,4),(15.7079632679489,
16.1780069365874,16.6725798287036,17.1671527208199,17.6617256129361,18.1562985050523,
18.6508713971686,19.1454442892848,19.6400171814011,20.1345900735173,20.6291629656336,
21.1237358577498,21.6183087498661,21.9911485751285),.UNSPECIFIED.);
#266=B_SPLINE_CURVE_WITH_KNOTS('',3,(#14024,#14025,#14026,#14027,#14028,
#14029,#14030,#14031,#14032,#14033,#14034,#14035,#14036,#14037,#14038,#14039,
#14040,#14041,#14042,#14043,#14044,#14045,#14046,#14047,#14048,#14049,#14050,
#14051,#14052,#14053,#14054),.UNSPECIFIED.,.F.,.F.,(4,3,3,3,3,3,3,3,3,3,
4),(0.,0.0822466706468383,0.162608105240606,0.216579893838171,0.23924274204394,
0.301838371937517,0.36076250940623,0.388067588559334,0.409537377502954,
0.476290104322315,0.53753492181237),.UNSPECIFIED.);
#267=B_SPLINE_CURVE_WITH_KNOTS('',3,(#14055,#14056,#14057,#14058,#14059,
#14060,#14061,#14062,#14063,#14064,#14065,#14066,#14067,#14068,#14069,#14070,
#14071,#14072,#14073,#14074,#14075,#14076,#14077,#14078,#14079,#14080,#14081,
#14082),.UNSPECIFIED.,.F.,.F.,(4,3,3,3,3,3,3,3,3,4),(0.,0.0665230127441691,
0.13429495842692,0.176258819244205,0.195926107024299,0.263526952009386,
0.33682854572103,0.365338415901403,0.449700157257057,0.534061898612711),
 .UNSPECIFIED.);
#268=B_SPLINE_CURVE_WITH_KNOTS('',3,(#14083,#14084,#14085,#14086,#14087,
#14088,#14089,#14090,#14091,#14092,#14093,#14094,#14095,#14096,#14097,#14098,
#14099,#14100,#14101,#14102,#14103,#14104,#14105,#14106,#14107,#14108,#14109,
#14110,#14111,#14112,#14113,#14114,#14115,#14116,#14117,#14118,#14119,#14120,
#14121,#14122),.UNSPECIFIED.,.F.,.F.,(4,3,3,3,3,3,3,3,3,3,3,3,3,4),(-53.8258642502287,
-53.4138723485545,-52.9192994564383,-52.424726564322,-51.9301536722058,
-51.4355807800895,-50.9410078879733,-50.446434995857,-49.9518621037408,
-49.4572892116245,-48.9627163195083,-48.4681434273921,-47.9735705352758,
-47.5426789430491),.UNSPECIFIED.);
#269=B_SPLINE_CURVE_WITH_KNOTS('',3,(#14584,#14585,#14586,#14587,#14588,
#14589,#14590,#14591,#14592,#14593,#14594,#14595,#14596,#14597,#14598,#14599,
#14600,#14601,#14602,#14603,#14604,#14605,#14606,#14607,#14608,#14609,#14610,
#14611),.UNSPECIFIED.,.F.,.F.,(4,3,3,3,3,3,3,3,3,4),(0.,0.0665230199567328,
0.134294967830964,0.176258831509978,0.195926124443112,0.263526952009376,
0.336828549458816,0.365338416771381,0.449700157692121,0.534061898612861),
 .UNSPECIFIED.);
#270=B_SPLINE_CURVE_WITH_KNOTS('',3,(#14612,#14613,#14614,#14615,#14616,
#14617,#14618,#14619,#14620,#14621,#14622,#14623,#14624,#14625,#14626,#14627,
#14628,#14629,#14630,#14631,#14632,#14633,#14634,#14635,#14636,#14637,#14638,
#14639,#14640,#14641,#14642),.UNSPECIFIED.,.F.,.F.,(4,3,3,3,3,3,3,3,3,3,
4),(50.7845845730308,50.9410078879733,51.4355807800895,51.9301536722058,
52.424726564322,52.9192994564383,53.4138723485545,53.9084452406708,54.403018132787,
54.8975910249033,55.3921639170195),.UNSPECIFIED.);
#271=B_SPLINE_CURVE_WITH_KNOTS('',3,(#14643,#14644,#14645,#14646,#14647,
#14648,#14649,#14650,#14651,#14652,#14653,#14654,#14655,#14656,#14657,#14658,
#14659,#14660,#14661,#14662,#14663,#14664,#14665,#14666,#14667,#14668,#14669,
#14670,#14671,#14672,#14673),.UNSPECIFIED.,.F.,.F.,(4,3,3,3,3,3,3,3,3,3,
4),(0.,0.0822466663612967,0.162608100396307,0.216579890867136,0.239242742625966,
0.301838371937549,0.360762509406336,0.388067584071394,0.409537375230468,
0.476290092032249,0.537534921812695),.UNSPECIFIED.);
#272=B_SPLINE_CURVE_WITH_KNOTS('',3,(#14873,#14874,#14875,#14876,#14877,
#14878,#14879,#14880,#14881,#14882,#14883,#14884,#14885,#14886,#14887,#14888,
#14889,#14890,#14891),.UNSPECIFIED.,.F.,.F.,(4,3,3,3,3,3,4),(-3.69871549170445,
-3.49775346748116,-2.99807440069814,-2.49839533391511,-1.99871626713209,
-1.49903720034907,-1.00018350866767),.UNSPECIFIED.);
#273=B_SPLINE_CURVE_WITH_KNOTS('',3,(#14894,#14895,#14896,#14897),
 .UNSPECIFIED.,.F.,.F.,(4,4),(0.,0.443060670554495),.UNSPECIFIED.);
#274=B_SPLINE_CURVE_WITH_KNOTS('',3,(#14902,#14903,#14904,#14905,#14906,
#14907,#14908,#14909,#14910,#14911,#14912,#14913,#14914,#14915,#14916,#14917,
#14918,#14919,#14920,#14921,#14922,#14923,#14924,#14925,#14926,#14927,#14928,
#14929,#14930,#14931,#14932,#14933,#14934,#14935,#14936,#14937,#14938,#14939,
#14940,#14941),.UNSPECIFIED.,.F.,.F.,(4,3,3,3,3,3,3,3,3,3,3,3,3,4),(-9.98190079888403,
-9.49390226887744,-8.99422320209442,-8.4945441353114,-7.99486506852837,
-7.49518600174535,-6.99550693496233,-6.4958278681793,-5.99614880139628,
-5.49646973461325,-4.99679066783023,-4.49711160104721,-3.99743253426419,
-3.69871549170445),.UNSPECIFIED.);
#275=B_SPLINE_CURVE_WITH_KNOTS('',3,(#14942,#14943,#14944,#14945,#14946,
#14947,#14948,#14949,#14950,#14951,#14952,#14953,#14954,#14955,#14956,#14957,
#14958,#14959,#14960,#14961,#14962,#14963,#14964,#14965,#14966,#14967,#14968,
#14969,#14970,#14971,#14972,#14973,#14974,#14975,#14976,#14977,#14978,#14979,
#14980,#14981,#14982,#14983,#14984),.UNSPECIFIED.,.F.,.F.,(4,3,3,3,3,3,
3,3,3,3,3,3,3,3,4),(0.443060670554495,0.49967906678306,0.999358133566079,
1.4990372003491,1.99871626713212,2.49839533391514,2.99807440069816,3.49775346748117,
3.99743253426419,4.49711160104721,4.99679066783023,5.49646973461325,5.99614880139627,
6.49582786817929,6.72624597773408),.UNSPECIFIED.);
#276=B_SPLINE_CURVE_WITH_KNOTS('',3,(#14989,#14990,#14991,#14992,#14993,
#14994,#14995,#14996,#14997,#14998,#14999,#15000,#15001,#15002,#15003,#15004,
#15005,#15006,#15007,#15008,#15009,#15010,#15011,#15012,#15013,#15014,#15015,
#15016,#15017,#15018,#15019,#15020,#15021,#15022,#15023,#15024,#15025,#15026,
#15027,#15028,#15029,#15030,#15031),.UNSPECIFIED.,.F.,.F.,(4,3,3,3,3,3,
3,3,3,3,3,3,3,3,4),(-16.2650861060636,-15.9897301370567,-15.4900510702737,
-14.9903720034907,-14.4906929367077,-13.9910138699247,-13.4913348031416,
-12.9916557363586,-12.4919766695756,-11.9922976027926,-11.4926185360095,
-10.9929394692265,-10.4932604024435,-9.99358133566046,-9.98190079888403),
 .UNSPECIFIED.);
#277=B_SPLINE_CURVE_WITH_KNOTS('',3,(#15032,#15033,#15034,#15035,#15036,
#15037,#15038,#15039,#15040,#15041,#15042,#15043,#15044,#15045,#15046,#15047,
#15048,#15049,#15050,#15051,#15052,#15053,#15054,#15055,#15056,#15057,#15058,
#15059,#15060,#15061,#15062,#15063,#15064,#15065,#15066,#15067,#15068,#15069,
#15070,#15071,#15072,#15073,#15074),.UNSPECIFIED.,.F.,.F.,(4,3,3,3,3,3,
3,3,3,3,3,3,3,3,4),(6.72624597773408,6.99550693496231,7.49518600174534,
7.99486506852837,8.49454413531139,8.99422320209442,9.49390226887745,9.99358133566048,
10.4932604024435,10.9929394692265,11.4926185360096,11.9922976027926,12.4919766695756,
12.9916557363586,13.0094312849137),.UNSPECIFIED.);
#278=B_SPLINE_CURVE_WITH_KNOTS('',3,(#15079,#15080,#15081,#15082,#15083,
#15084,#15085,#15086,#15087,#15088,#15089,#15090,#15091,#15092,#15093,#15094,
#15095,#15096,#15097,#15098,#15099,#15100,#15101,#15102,#15103,#15104,#15105,
#15106,#15107,#15108,#15109,#15110,#15111,#15112,#15113,#15114,#15115,#15116,
#15117,#15118,#15119,#15120,#15121),.UNSPECIFIED.,.F.,.F.,(4,3,3,3,3,3,
3,3,3,3,3,3,3,3,4),(-22.5482714132432,-22.485558005236,-21.985878938453,
-21.48619987167,-20.986520804887,-20.486841738104,-19.9871626713209,-19.4874836045379,
-18.9878045377549,-18.4881254709719,-17.9884464041888,-17.4887673374058,
-16.9890882706228,-16.4894092038398,-16.2650861060636),.UNSPECIFIED.);
#279=B_SPLINE_CURVE_WITH_KNOTS('',3,(#15122,#15123,#15124,#15125,#15126,
#15127,#15128,#15129,#15130,#15131,#15132,#15133,#15134,#15135,#15136,#15137,
#15138,#15139,#15140,#15141,#15142,#15143,#15144,#15145,#15146,#15147,#15148,
#15149,#15150,#15151,#15152,#15153,#15154,#15155,#15156,#15157,#15158,#15159,
#15160,#15161),.UNSPECIFIED.,.F.,.F.,(4,3,3,3,3,3,3,3,3,3,3,3,3,4),(13.0094312849137,
13.4913348031417,13.9910138699247,14.4906929367077,14.9903720034907,15.4900510702737,
15.9897301370568,16.4894092038398,16.9890882706228,17.4887673374058,17.9884464041888,
18.4881254709718,18.9878045377549,19.2926165920933),.UNSPECIFIED.);
#280=B_SPLINE_CURVE_WITH_KNOTS('',3,(#15166,#15167,#15168,#15169,#15170,
#15171,#15172,#15173,#15174,#15175,#15176,#15177,#15178,#15179,#15180,#15181,
#15182,#15183,#15184,#15185,#15186,#15187,#15188,#15189,#15190,#15191,#15192,
#15193,#15194,#15195,#15196,#15197,#15198,#15199,#15200,#15201,#15202,#15203,
#15204,#15205),.UNSPECIFIED.,.F.,.F.,(4,3,3,3,3,3,3,3,3,3,3,3,3,4),(-28.8314567204228,
-28.4817068066323,-27.9820277398493,-27.4823486730663,-26.9826696062833,
-26.4829905395002,-25.9833114727172,-25.4836324059342,-24.9839533391512,
-24.4842742723681,-23.9845952055851,-23.4849161388021,-22.9852370720191,
-22.5482714132432),.UNSPECIFIED.);
#281=B_SPLINE_CURVE_WITH_KNOTS('',3,(#15206,#15207,#15208,#15209,#15210,
#15211,#15212,#15213,#15214,#15215,#15216,#15217,#15218,#15219,#15220,#15221,
#15222,#15223,#15224,#15225,#15226,#15227,#15228,#15229,#15230,#15231,#15232,
#15233,#15234,#15235,#15236,#15237,#15238,#15239,#15240,#15241,#15242,#15243,
#15244,#15245,#15246,#15247,#15248),.UNSPECIFIED.,.F.,.F.,(4,3,3,3,3,3,
3,3,3,3,3,3,3,3,4),(19.2926165920933,19.4874836045379,19.9871626713209,
20.4868417381039,20.986520804887,21.48619987167,21.985878938453,22.4855580052361,
22.9852370720191,23.4849161388021,23.9845952055851,24.4842742723682,24.9839533391512,
25.4836324059342,25.5758018992728),.UNSPECIFIED.);
#282=B_SPLINE_CURVE_WITH_KNOTS('',3,(#15253,#15254,#15255,#15256,#15257,
#15258,#15259,#15260,#15261,#15262,#15263,#15264,#15265,#15266,#15267,#15268,
#15269,#15270,#15271,#15272,#15273,#15274,#15275,#15276,#15277,#15278,#15279,
#15280,#15281,#15282,#15283,#15284,#15285,#15286,#15287,#15288,#15289,#15290,
#15291,#15292,#15293,#15294,#15295),.UNSPECIFIED.,.F.,.F.,(4,3,3,3,3,3,
3,3,3,3,3,3,3,3,4),(-35.1146420276024,-34.9775346748116,-34.4778556080286,
-33.9781765412456,-33.4784974744626,-32.9788184076795,-32.4791393408965,
-31.9794602741135,-31.4797812073305,-30.9801021405474,-30.4804230737644,
-29.9807440069814,-29.4810649401984,-28.9813858734153,-28.8314567204228),
 .UNSPECIFIED.);
#283=B_SPLINE_CURVE_WITH_KNOTS('',3,(#15296,#15297,#15298,#15299,#15300,
#15301,#15302,#15303,#15304,#15305,#15306,#15307,#15308,#15309,#15310,#15311,
#15312,#15313,#15314,#15315,#15316,#15317,#15318,#15319,#15320,#15321,#15322,
#15323,#15324,#15325,#15326,#15327,#15328,#15329,#15330,#15331,#15332,#15333,
#15334,#15335),.UNSPECIFIED.,.F.,.F.,(4,3,3,3,3,3,3,3,3,3,3,3,3,4),(25.5758018992728,
25.9833114727172,26.4829905395003,26.9826696062833,27.4823486730663,27.9820277398493,
28.4817068066324,28.9813858734154,29.4810649401984,29.9807440069814,30.4804230737645,
30.9801021405475,31.4797812073305,31.8589872064524),.UNSPECIFIED.);
#284=B_SPLINE_CURVE_WITH_KNOTS('',3,(#15340,#15341,#15342,#15343,#15344,
#15345,#15346,#15347,#15348,#15349,#15350,#15351,#15352,#15353,#15354,#15355,
#15356,#15357,#15358,#15359,#15360,#15361,#15362,#15363,#15364,#15365,#15366,
#15367,#15368,#15369,#15370,#15371,#15372,#15373,#15374,#15375,#15376,#15377,
#15378,#15379),.UNSPECIFIED.,.F.,.F.,(4,3,3,3,3,3,3,3,3,3,3,3,3,4),(-41.397827334782,
-40.9736834762079,-40.4740044094249,-39.9743253426419,-39.4746462758588,
-38.9749672090758,-38.4752881422928,-37.9756090755098,-37.4759300087267,
-36.9762509419437,-36.4765718751607,-35.9768928083777,-35.4772137415947,
-35.1146420276024),.UNSPECIFIED.);
#285=B_SPLINE_CURVE_WITH_KNOTS('',3,(#15380,#15381,#15382,#15383,#15384,
#15385,#15386,#15387,#15388,#15389,#15390,#15391,#15392,#15393,#15394,#15395,
#15396,#15397,#15398,#15399,#15400,#15401,#15402,#15403,#15404,#15405,#15406,
#15407,#15408,#15409,#15410,#15411,#15412,#15413,#15414,#15415,#15416,#15417,
#15418,#15419,#15420,#15421,#15422),.UNSPECIFIED.,.F.,.F.,(4,3,3,3,3,3,
3,3,3,3,3,3,3,3,4),(31.8589872064524,31.9794602741135,32.4791393408966,
32.9788184076796,33.4784974744626,33.9781765412456,34.4778556080286,34.9775346748117,
35.4772137415947,35.9768928083777,36.4765718751607,36.9762509419437,37.4759300087267,
37.9756090755098,38.142172513632),.UNSPECIFIED.);
#286=B_SPLINE_CURVE_WITH_KNOTS('',3,(#15427,#15428,#15429,#15430,#15431,
#15432,#15433,#15434,#15435,#15436,#15437,#15438,#15439,#15440,#15441,#15442,
#15443,#15444,#15445,#15446,#15447,#15448,#15449,#15450,#15451,#15452,#15453,
#15454,#15455,#15456,#15457,#15458,#15459,#15460,#15461,#15462,#15463,#15464,
#15465,#15466,#15467,#15468,#15469),.UNSPECIFIED.,.F.,.F.,(4,3,3,3,3,3,
3,3,3,3,3,3,3,3,4),(-47.6810126419616,-47.4695113443872,-46.9698322776042,
-46.4701532108212,-45.9704741440381,-45.4707950772551,-44.9711160104721,
-44.4714369436891,-43.971757876906,-43.472078810123,-42.97239974334,-42.472720676557,
-41.973041609774,-41.4733625429909,-41.397827334782),.UNSPECIFIED.);
#287=B_SPLINE_CURVE_WITH_KNOTS('',3,(#15470,#15471,#15472,#15473,#15474,
#15475,#15476,#15477,#15478,#15479,#15480,#15481,#15482,#15483,#15484,#15485,
#15486,#15487,#15488,#15489,#15490,#15491,#15492,#15493,#15494,#15495,#15496,
#15497,#15498,#15499,#15500,#15501,#15502,#15503,#15504,#15505,#15506,#15507,
#15508,#15509),.UNSPECIFIED.,.F.,.F.,(4,3,3,3,3,3,3,3,3,3,3,3,3,4),(38.142172513632,
38.4752881422928,38.9749672090758,39.4746462758589,39.9743253426419,40.4740044094249,
40.973683476208,41.473362542991,41.973041609774,42.472720676557,42.9723997433401,
43.4720788101231,43.9717578769061,44.4253578208116),.UNSPECIFIED.);
#288=B_SPLINE_CURVE_WITH_KNOTS('',3,(#15514,#15515,#15516,#15517,#15518,
#15519,#15520,#15521,#15522,#15523,#15524,#15525,#15526,#15527,#15528,#15529,
#15530,#15531,#15532,#15533,#15534,#15535,#15536,#15537,#15538,#15539,#15540,
#15541),.UNSPECIFIED.,.F.,.F.,(4,3,3,3,3,3,3,3,3,4),(-53.9641979491412,
-52.9659810790005,-51.9666229454344,-50.9672648118684,-49.9679066783023,
-49.4682276115193,-48.9685485447363,-48.4688694779533,-47.9691904111702,
-47.6810126419616),.UNSPECIFIED.);
#289=B_SPLINE_CURVE_WITH_KNOTS('',3,(#15542,#15543,#15544,#15545,#15546,
#15547,#15548,#15549,#15550,#15551,#15552,#15553,#15554,#15555,#15556,#15557,
#15558,#15559,#15560,#15561,#15562,#15563,#15564,#15565,#15566,#15567,#15568,
#15569,#15570,#15571,#15572,#15573,#15574,#15575,#15576,#15577,#15578,#15579,
#15580,#15581),.UNSPECIFIED.,.F.,.F.,(4,3,3,3,3,3,3,3,3,3,3,3,3,4),(44.4253578208116,
44.4714369436892,44.9711160104722,45.4707950772552,45.9704741440382,46.4701532108212,
46.9698322776042,47.4695113443873,47.9691904111703,48.4688694779533,48.9685485447363,
49.4682276115193,49.9679066783024,50.7085431279912),.UNSPECIFIED.);
#290=B_SPLINE_CURVE_WITH_KNOTS('',3,(#15586,#15587,#15588,#15589,#15590,
#15591,#15592,#15593,#15594,#15595,#15596,#15597,#15598,#15599,#15600,#15601,
#15602,#15603,#15604,#15605,#15606,#15607),.UNSPECIFIED.,.F.,.F.,(4,3,3,
3,3,3,3,4),(-60.2473832563207,-59.9614880139628,-58.9621298803968,-57.9627717468307,
-56.9634136132647,-55.9640554796986,-54.9646973461326,-53.9641979491412),
 .UNSPECIFIED.);
#291=B_SPLINE_CURVE_WITH_KNOTS('',3,(#15608,#15609,#15610,#15611,#15612,
#15613,#15614,#15615,#15616,#15617,#15618,#15619,#15620,#15621,#15622,#15623,
#15624,#15625,#15626,#15627,#15628,#15629,#15630,#15631,#15632),
 .UNSPECIFIED.,.F.,.F.,(4,3,3,3,3,3,3,3,4),(50.7085431279912,50.9672648118684,
51.9666229454345,52.9659810790005,53.9653392125666,54.9646973461326,55.9640554796987,
56.9634136132647,56.9917284351708),.UNSPECIFIED.);
#292=B_SPLINE_CURVE_WITH_KNOTS('',3,(#15637,#15638,#15639,#15640,#15641,
#15642,#15643,#15644,#15645,#15646,#15647,#15648,#15649,#15650,#15651,#15652,
#15653,#15654,#15655,#15656,#15657,#15658),.UNSPECIFIED.,.F.,.F.,(4,3,3,
3,3,3,3,4),(-66.5305685635003,-65.9576368153591,-64.958278681793,-63.958920548227,
-62.9595624146609,-61.9602042810949,-60.9608461475288,-60.2473832563207),
 .UNSPECIFIED.);
#293=B_SPLINE_CURVE_WITH_KNOTS('',3,(#15659,#15660,#15661,#15662,#15663,
#15664,#15665,#15666,#15667,#15668,#15669,#15670,#15671,#15672,#15673,#15674,
#15675,#15676,#15677,#15678,#15679,#15680),.UNSPECIFIED.,.F.,.F.,(4,3,3,
3,3,3,3,4),(56.9917284351708,57.9627717468308,58.9621298803968,59.9614880139629,
60.9608461475289,61.960204281095,62.959562414661,63.2749137423504),
 .UNSPECIFIED.);
#294=B_SPLINE_CURVE_WITH_KNOTS('',3,(#15685,#15686,#15687,#15688,#15689,
#15690,#15691,#15692,#15693,#15694,#15695,#15696,#15697,#15698,#15699,#15700,
#15701,#15702,#15703,#15704,#15705,#15706),.UNSPECIFIED.,.F.,.F.,(4,3,3,
3,3,3,3,4),(-72.8137538706799,-71.9537856167554,-70.9544274831893,-69.9550693496233,
-68.9557112160572,-67.9563530824912,-66.9569949489251,-66.5305685635003),
 .UNSPECIFIED.);
#295=B_SPLINE_CURVE_WITH_KNOTS('',3,(#15707,#15708,#15709,#15710,#15711,
#15712,#15713,#15714,#15715,#15716,#15717,#15718,#15719,#15720,#15721,#15722,
#15723,#15724,#15725,#15726,#15727,#15728),.UNSPECIFIED.,.F.,.F.,(4,3,3,
3,3,3,3,4),(63.2749137423504,63.958920548227,64.9582786817931,65.9576368153591,
66.9569949489252,67.9563530824912,68.9557112160573,69.55809904953),
 .UNSPECIFIED.);
#296=B_SPLINE_CURVE_WITH_KNOTS('',3,(#15733,#15734,#15735,#15736,#15737,
#15738,#15739,#15740,#15741,#15742,#15743,#15744,#15745,#15746,#15747,#15748,
#15749,#15750,#15751,#15752,#15753,#15754,#15755,#15756,#15757),
 .UNSPECIFIED.,.F.,.F.,(4,3,3,3,3,3,3,3,4),(-79.0969391778595,-78.9492925517177,
-77.9499344181516,-76.9505762845856,-75.9512181510195,-74.9518600174535,
-73.9525018838875,-72.9531437503214,-72.8137538706799),.UNSPECIFIED.);
#297=B_SPLINE_CURVE_WITH_KNOTS('',3,(#15758,#15759,#15760,#15761,#15762,
#15763,#15764,#15765,#15766,#15767,#15768,#15769,#15770,#15771,#15772,#15773,
#15774,#15775,#15776,#15777,#15778,#15779),.UNSPECIFIED.,.F.,.F.,(4,3,3,
3,3,3,3,4),(69.55809904953,69.9550693496233,70.9544274831893,71.9537856167554,
72.9531437503215,73.9525018838875,74.9518600174536,75.8412843567096),
 .UNSPECIFIED.);
#298=B_SPLINE_CURVE_WITH_KNOTS('',3,(#15784,#15785,#15786,#15787,#15788,
#15789,#15790,#15791,#15792,#15793,#15794,#15795,#15796,#15797,#15798,#15799,
#15800,#15801,#15802,#15803,#15804,#15805),.UNSPECIFIED.,.F.,.F.,(4,3,3,
3,3,3,3,4),(-85.3801244850391,-84.945441353114,-83.9460832195479,-82.9467250859819,
-81.9473669524158,-80.9480088188498,-79.9486506852837,-79.0969391778595),
 .UNSPECIFIED.);
#299=B_SPLINE_CURVE_WITH_KNOTS('',3,(#15806,#15807,#15808,#15809,#15810,
#15811,#15812,#15813,#15814,#15815,#15816,#15817,#15818,#15819,#15820,#15821,
#15822,#15823,#15824,#15825,#15826,#15827,#15828,#15829,#15830),
 .UNSPECIFIED.,.F.,.F.,(4,3,3,3,3,3,3,3,4),(75.8412843567096,75.9512181510196,
76.9505762845857,77.9499344181517,78.9492925517178,79.9486506852838,80.9480088188499,
81.9473669524159,82.1244696638892),.UNSPECIFIED.);
#300=B_SPLINE_CURVE_WITH_KNOTS('',3,(#15835,#15836,#15837,#15838,#15839,
#15840,#15841,#15842,#15843,#15844,#15845,#15846,#15847,#15848,#15849,#15850,
#15851,#15852,#15853,#15854,#15855,#15856),.UNSPECIFIED.,.F.,.F.,(4,3,3,
3,3,3,3,4),(-91.6633097922187,-90.9415901545102,-89.9422320209442,-88.9428738873782,
-87.9435157538121,-86.944157620246,-85.94479948668,-85.3801244850391),
 .UNSPECIFIED.);
#301=B_SPLINE_CURVE_WITH_KNOTS('',3,(#15857,#15858,#15859,#15860,#15861,
#15862,#15863,#15864,#15865,#15866,#15867,#15868,#15869,#15870,#15871,#15872,
#15873,#15874,#15875,#15876,#15877,#15878),.UNSPECIFIED.,.F.,.F.,(4,3,3,
3,3,3,3,4),(82.1244696638892,82.946725085982,83.946083219548,84.9454413531141,
85.9447994866801,86.9441576202461,87.9435157538122,88.4076549710687),
 .UNSPECIFIED.);
#302=B_SPLINE_CURVE_WITH_KNOTS('',3,(#15883,#15884,#15885,#15886,#15887,
#15888,#15889,#15890,#15891,#15892,#15893,#15894,#15895,#15896,#15897,#15898,
#15899,#15900,#15901,#15902,#15903,#15904,#15905,#15906,#15907),
 .UNSPECIFIED.,.F.,.F.,(4,3,3,3,3,3,3,3,4),(-97.9464950993983,-97.9370970894726,
-96.9377389559065,-95.9383808223405,-94.9390226887744,-93.9396645552084,
-92.9403064216423,-91.9409482880763,-91.6633097922187),.UNSPECIFIED.);
#303=B_SPLINE_CURVE_WITH_KNOTS('',3,(#15908,#15909,#15910,#15911,#15912,
#15913,#15914,#15915,#15916,#15917,#15918,#15919,#15920,#15921,#15922,#15923,
#15924,#15925,#15926,#15927,#15928,#15929),.UNSPECIFIED.,.F.,.F.,(4,3,3,
3,3,3,3,4),(88.4076549710687,88.9428738873782,89.9422320209442,90.9415901545103,
91.9409482880763,92.9403064216424,93.9396645552084,94.6908402782483),
 .UNSPECIFIED.);
#304=B_SPLINE_CURVE_WITH_KNOTS('',3,(#15934,#15935,#15936,#15937,#15938,
#15939,#15940,#15941,#15942,#15943,#15944,#15945,#15946,#15947,#15948,#15949,
#15950,#15951,#15952,#15953,#15954,#15955),.UNSPECIFIED.,.F.,.F.,(4,3,3,
3,3,3,3,4),(-104.229680406578,-103.933245890869,-102.933887757303,-101.934529623737,
-100.935171490171,-99.9358133566047,-98.9364552230386,-97.9464950993983),
 .UNSPECIFIED.);
#305=B_SPLINE_CURVE_WITH_KNOTS('',3,(#15956,#15957,#15958,#15959,#15960,
#15961,#15962,#15963,#15964,#15965,#15966,#15967,#15968,#15969,#15970,#15971,
#15972,#15973,#15974,#15975,#15976,#15977,#15978,#15979,#15980),
 .UNSPECIFIED.,.F.,.F.,(4,3,3,3,3,3,3,3,4),(94.6908402782483,94.9390226887745,
95.9383808223405,96.9377389559065,97.9370970894726,98.9364552230386,99.9358133566047,
100.935171490171,100.974025585428),.UNSPECIFIED.);
#306=B_SPLINE_CURVE_WITH_KNOTS('',3,(#15985,#15986,#15987,#15988,#15989,
#15990,#15991,#15992,#15993,#15994,#15995,#15996,#15997,#15998,#15999,#16000,
#16001,#16002,#16003,#16004,#16005,#16006),.UNSPECIFIED.,.F.,.F.,(4,3,3,
3,3,3,3,4),(-110.512865713757,-109.929394692265,-108.930036558699,-107.930678425133,
-106.931320291567,-105.931962158001,-104.932604024435,-104.229680406578),
 .UNSPECIFIED.);
#307=B_SPLINE_CURVE_WITH_KNOTS('',3,(#16007,#16008,#16009,#16010,#16011,
#16012,#16013,#16014,#16015,#16016,#16017,#16018,#16019,#16020,#16021,#16022,
#16023,#16024,#16025,#16026,#16027,#16028),.UNSPECIFIED.,.F.,.F.,(4,3,3,
3,3,3,3,4),(100.974025585428,101.934529623737,102.933887757303,103.933245890869,
104.932604024435,105.931962158001,106.931320291567,107.257210892608),
 .UNSPECIFIED.);
#308=B_SPLINE_CURVE_WITH_KNOTS('',3,(#16033,#16034,#16035,#16036,#16037,
#16038,#16039,#16040,#16041,#16042,#16043,#16044,#16045,#16046,#16047,#16048,
#16049,#16050,#16051,#16052,#16053,#16054),.UNSPECIFIED.,.F.,.F.,(4,3,3,
3,3,3,3,4),(-116.796051020937,-115.925543493661,-114.926185360095,-113.926827226529,
-112.927469092963,-111.928110959397,-110.928752825831,-110.512865713757),
 .UNSPECIFIED.);
#309=B_SPLINE_CURVE_WITH_KNOTS('',3,(#16055,#16056,#16057,#16058,#16059,
#16060,#16061,#16062,#16063,#16064,#16065,#16066,#16067,#16068,#16069,#16070,
#16071,#16072,#16073,#16074,#16075,#16076),.UNSPECIFIED.,.F.,.F.,(4,3,3,
3,3,3,3,4),(107.257210892608,107.930678425133,108.930036558699,109.929394692265,
110.928752825831,111.928110959397,112.927469092963,113.540396199787),
 .UNSPECIFIED.);
#310=B_SPLINE_CURVE_WITH_KNOTS('',3,(#16081,#16082,#16083,#16084,#16085,
#16086,#16087,#16088,#16089,#16090,#16091,#16092,#16093,#16094,#16095,#16096,
#16097,#16098,#16099,#16100,#16101,#16102,#16103,#16104,#16105),
 .UNSPECIFIED.,.F.,.F.,(4,3,3,3,3,3,3,3,4),(-123.079236328117,-122.921050428624,
-121.921692295058,-120.922334161492,-119.922976027926,-118.92361789436,
-117.924259760793,-116.924901627227,-116.796051020937),.UNSPECIFIED.);
#311=B_SPLINE_CURVE_WITH_KNOTS('',3,(#16106,#16107,#16108,#16109,#16110,
#16111,#16112,#16113,#16114,#16115,#16116,#16117,#16118,#16119,#16120,#16121,
#16122,#16123,#16124,#16125,#16126,#16127),.UNSPECIFIED.,.F.,.F.,(4,3,3,
3,3,3,3,4),(113.540396199787,113.926827226529,114.926185360095,115.925543493661,
116.924901627228,117.924259760794,118.92361789436,119.823581506967),
 .UNSPECIFIED.);
#312=B_SPLINE_CURVE_WITH_KNOTS('',3,(#16132,#16133,#16134,#16135,#16136,
#16137,#16138,#16139,#16140,#16141,#16142,#16143,#16144,#16145,#16146,#16147,
#16148,#16149,#16150,#16151,#16152,#16153),.UNSPECIFIED.,.F.,.F.,(4,3,3,
3,3,3,3,4),(-129.362421635296,-128.91719923002,-127.917841096454,-126.918482962888,
-125.919124829322,-124.919766695756,-123.92040856219,-123.079236328117),
 .UNSPECIFIED.);
#313=B_SPLINE_CURVE_WITH_KNOTS('',3,(#16154,#16155,#16156,#16157,#16158,
#16159,#16160,#16161,#16162,#16163,#16164,#16165,#16166,#16167,#16168,#16169,
#16170,#16171,#16172,#16173,#16174,#16175,#16176,#16177,#16178),
 .UNSPECIFIED.,.F.,.F.,(4,3,3,3,3,3,3,3,4),(119.823581506967,119.922976027926,
120.922334161492,121.921692295058,122.921050428624,123.92040856219,124.919766695756,
125.919124829322,126.106766814146),.UNSPECIFIED.);
#314=B_SPLINE_CURVE_WITH_KNOTS('',3,(#16183,#16184,#16185,#16186,#16187,
#16188,#16189,#16190,#16191,#16192,#16193,#16194,#16195,#16196,#16197,#16198,
#16199,#16200,#16201,#16202,#16203,#16204),.UNSPECIFIED.,.F.,.F.,(4,3,3,
3,3,3,3,4),(-135.645606942476,-134.913348031416,-133.91398989785,-132.914631764284,
-131.915273630718,-130.915915497152,-129.916557363586,-129.362421635296),
 .UNSPECIFIED.);
#315=B_SPLINE_CURVE_WITH_KNOTS('',3,(#16205,#16206,#16207,#16208,#16209,
#16210,#16211,#16212,#16213,#16214,#16215,#16216,#16217,#16218,#16219,#16220,
#16221,#16222,#16223,#16224,#16225,#16226),.UNSPECIFIED.,.F.,.F.,(4,3,3,
3,3,3,3,4),(126.106766814146,126.918482962888,127.917841096454,128.91719923002,
129.916557363586,130.915915497152,131.915273630718,132.389952121326),
 .UNSPECIFIED.);
#316=B_SPLINE_CURVE_WITH_KNOTS('',3,(#16231,#16232,#16233,#16234,#16235,
#16236,#16237,#16238,#16239,#16240,#16241,#16242,#16243,#16244,#16245,#16246,
#16247,#16248,#16249,#16250,#16251,#16252,#16253,#16254,#16255),
 .UNSPECIFIED.,.F.,.F.,(4,3,3,3,3,3,3,3,4),(-141.928792249655,-141.908854966379,
-140.909496832813,-139.910138699247,-138.91078056568,-137.911422432114,
-136.912064298548,-135.912706164982,-135.645606942476),.UNSPECIFIED.);
#317=B_SPLINE_CURVE_WITH_KNOTS('',3,(#16256,#16257,#16258,#16259,#16260,
#16261,#16262,#16263,#16264,#16265,#16266,#16267,#16268,#16269,#16270,#16271,
#16272,#16273,#16274,#16275,#16276,#16277),.UNSPECIFIED.,.F.,.F.,(4,3,3,
3,3,3,3,4),(132.389952121326,132.914631764284,133.91398989785,134.913348031416,
135.912706164982,136.912064298549,137.911422432115,138.673137428505),
 .UNSPECIFIED.);
#318=B_SPLINE_CURVE_WITH_KNOTS('',3,(#16282,#16283,#16284,#16285,#16286,
#16287,#16288,#16289,#16290,#16291,#16292,#16293,#16294,#16295,#16296,#16297,
#16298,#16299,#16300,#16301,#16302,#16303),.UNSPECIFIED.,.F.,.F.,(4,3,3,
3,3,3,3,4),(-148.211977556835,-147.905003767775,-146.905645634209,-145.906287500643,
-144.906929367077,-143.907571233511,-142.908213099945,-141.928792249655),
 .UNSPECIFIED.);
#319=B_SPLINE_CURVE_WITH_KNOTS('',3,(#16304,#16305,#16306,#16307,#16308,
#16309,#16310,#16311,#16312,#16313,#16314,#16315,#16316,#16317,#16318,#16319,
#16320,#16321,#16322,#16323,#16324,#16325,#16326,#16327,#16328),
 .UNSPECIFIED.,.F.,.F.,(4,3,3,3,3,3,3,3,4),(138.673137428505,138.910780565681,
139.910138699247,140.909496832813,141.908854966379,142.908213099945,143.907571233511,
144.906929367077,144.956322735685),.UNSPECIFIED.);
#320=B_SPLINE_CURVE_WITH_KNOTS('',3,(#16333,#16334,#16335,#16336,#16337,
#16338,#16339,#16340,#16341,#16342,#16343,#16344,#16345,#16346,#16347,#16348,
#16349,#16350,#16351,#16352,#16353,#16354),.UNSPECIFIED.,.F.,.F.,(4,3,3,
3,3,3,3,4),(-154.495162864015,-153.901152569171,-152.901794435605,-151.902436302039,
-150.903078168473,-149.903720034907,-148.904361901341,-148.211977556835),
 .UNSPECIFIED.);
#321=B_SPLINE_CURVE_WITH_KNOTS('',3,(#16355,#16356,#16357,#16358,#16359,
#16360,#16361,#16362,#16363,#16364,#16365,#16366,#16367,#16368,#16369,#16370,
#16371,#16372,#16373,#16374,#16375,#16376),.UNSPECIFIED.,.F.,.F.,(4,3,3,
3,3,3,3,4),(144.956322735685,145.906287500643,146.905645634209,147.905003767775,
148.904361901341,149.903720034907,150.903078168473,151.239508042865),
 .UNSPECIFIED.);
#322=B_SPLINE_CURVE_WITH_KNOTS('',3,(#16381,#16382,#16383,#16384,#16385,
#16386,#16387,#16388,#16389,#16390,#16391,#16392,#16393,#16394,#16395,#16396,
#16397,#16398,#16399,#16400,#16401,#16402),.UNSPECIFIED.,.F.,.F.,(4,3,3,
3,3,3,3,4),(-160.778348171194,-159.897301370567,-158.897943237001,-157.898585103435,
-156.899226969869,-155.899868836303,-154.900510702737,-154.495162864015),
 .UNSPECIFIED.);
#323=B_SPLINE_CURVE_WITH_KNOTS('',3,(#16403,#16404,#16405,#16406,#16407,
#16408,#16409,#16410,#16411,#16412,#16413,#16414,#16415,#16416,#16417,#16418,
#16419,#16420,#16421,#16422,#16423,#16424),.UNSPECIFIED.,.F.,.F.,(4,3,3,
3,3,3,3,4),(151.239508042865,151.902436302039,152.901794435605,153.901152569171,
154.900510702737,155.899868836303,156.899226969869,157.522693350044),
 .UNSPECIFIED.);
#324=B_SPLINE_CURVE_WITH_KNOTS('',3,(#16429,#16430,#16431,#16432,#16433,
#16434,#16435,#16436,#16437,#16438,#16439,#16440,#16441,#16442,#16443,#16444,
#16445,#16446,#16447,#16448,#16449,#16450,#16451,#16452,#16453),
 .UNSPECIFIED.,.F.,.F.,(4,3,3,3,3,3,3,3,4),(-167.061533478374,-166.89280830553,
-165.893450171964,-164.894092038398,-163.894733904832,-162.895375771266,
-161.8960176377,-160.896659504134,-160.778348171194),.UNSPECIFIED.);
#325=B_SPLINE_CURVE_WITH_KNOTS('',3,(#16454,#16455,#16456,#16457,#16458,
#16459,#16460,#16461,#16462,#16463,#16464,#16465,#16466,#16467,#16468,#16469,
#16470,#16471,#16472,#16473,#16474,#16475),.UNSPECIFIED.,.F.,.F.,(4,3,3,
3,3,3,3,4),(157.522693350044,157.898585103435,158.897943237002,159.897301370568,
160.896659504134,161.8960176377,162.895375771266,163.805878657224),
 .UNSPECIFIED.);
#326=B_SPLINE_CURVE_WITH_KNOTS('',3,(#16480,#16481,#16482,#16483,#16484,
#16485,#16486,#16487,#16488,#16489,#16490,#16491,#16492,#16493,#16494,#16495,
#16496,#16497,#16498,#16499,#16500,#16501),.UNSPECIFIED.,.F.,.F.,(4,3,3,
3,3,3,3,4),(-173.344718785553,-172.888957106926,-171.88959897336,-170.890240839794,
-169.890882706228,-168.891524572662,-167.892166439096,-167.061533478374),
 .UNSPECIFIED.);
#327=B_SPLINE_CURVE_WITH_KNOTS('',3,(#16502,#16503,#16504,#16505,#16506,
#16507,#16508,#16509,#16510,#16511,#16512,#16513,#16514,#16515,#16516,#16517,
#16518,#16519,#16520,#16521,#16522,#16523,#16524,#16525,#16526),
 .UNSPECIFIED.,.F.,.F.,(4,3,3,3,3,3,3,3,4),(163.805878657224,163.894733904832,
164.894092038398,165.893450171964,166.89280830553,167.892166439096,168.891524572662,
169.890882706228,170.089063964403),.UNSPECIFIED.);
#328=B_SPLINE_CURVE_WITH_KNOTS('',3,(#16531,#16532,#16533,#16534,#16535,
#16536,#16537,#16538,#16539,#16540,#16541,#16542,#16543,#16544,#16545,#16546,
#16547,#16548,#16549,#16550,#16551,#16552),.UNSPECIFIED.,.F.,.F.,(4,3,3,
3,3,3,3,4),(-179.627904092733,-178.885105908322,-177.885747774756,-176.88638964119,
-175.887031507624,-174.887673374058,-173.888315240492,-173.344718785553),
 .UNSPECIFIED.);
#329=B_SPLINE_CURVE_WITH_KNOTS('',3,(#16553,#16554,#16555,#16556,#16557,
#16558,#16559,#16560,#16561,#16562,#16563,#16564,#16565,#16566,#16567,#16568,
#16569,#16570,#16571,#16572,#16573,#16574),.UNSPECIFIED.,.F.,.F.,(4,3,3,
3,3,3,3,4),(170.089063964403,170.890240839794,171.88959897336,172.888957106926,
173.888315240492,174.887673374058,175.887031507624,176.372249271583),
 .UNSPECIFIED.);
#330=B_SPLINE_CURVE_WITH_KNOTS('',3,(#16579,#16580,#16581,#16582,#16583,
#16584,#16585,#16586,#16587,#16588,#16589,#16590,#16591,#16592,#16593,#16594,
#16595,#16596,#16597,#16598,#16599,#16600,#16601,#16602,#16603),
 .UNSPECIFIED.,.F.,.F.,(4,3,3,3,3,3,3,3,4),(-185.911089399912,-185.880612843285,
-184.881254709719,-183.881896576153,-182.882538442587,-181.88318030902,
-180.883822175454,-179.884464041888,-179.627904092733),.UNSPECIFIED.);
#331=B_SPLINE_CURVE_WITH_KNOTS('',3,(#16604,#16605,#16606,#16607,#16608,
#16609,#16610,#16611,#16612,#16613,#16614,#16615,#16616,#16617,#16618,#16619,
#16620,#16621,#16622,#16623,#16624,#16625),.UNSPECIFIED.,.F.,.F.,(4,3,3,
3,3,3,3,4),(176.372249271583,176.88638964119,177.885747774756,178.885105908322,
179.884464041889,180.883822175455,181.883180309021,182.655434578762),
 .UNSPECIFIED.);
#332=B_SPLINE_CURVE_WITH_KNOTS('',3,(#16630,#16631,#16632,#16633,#16634,
#16635,#16636,#16637,#16638,#16639,#16640,#16641,#16642,#16643,#16644,#16645,
#16646,#16647,#16648,#16649,#16650,#16651),.UNSPECIFIED.,.F.,.F.,(4,3,3,
3,3,3,3,4),(-192.194274707092,-191.876761644681,-190.877403511115,-189.878045377549,
-188.878687243983,-187.879329110417,-186.879970976851,-185.911089399912),
 .UNSPECIFIED.);
#333=B_SPLINE_CURVE_WITH_KNOTS('',3,(#16652,#16653,#16654,#16655,#16656,
#16657,#16658,#16659,#16660,#16661,#16662,#16663,#16664,#16665,#16666,#16667,
#16668,#16669,#16670,#16671,#16672,#16673,#16674,#16675,#16676),
 .UNSPECIFIED.,.F.,.F.,(4,3,3,3,3,3,3,3,4),(182.655434578762,182.882538442587,
183.881896576153,184.881254709719,185.880612843285,186.879970976851,187.879329110417,
188.878687243983,188.938619885942),.UNSPECIFIED.);
#334=B_SPLINE_CURVE_WITH_KNOTS('',3,(#16681,#16682,#16683,#16684,#16685,
#16686,#16687,#16688,#16689,#16690,#16691,#16692,#16693,#16694,#16695,#16696,
#16697,#16698,#16699,#16700,#16701,#16702),.UNSPECIFIED.,.F.,.F.,(4,3,3,
3,3,3,3,4),(-198.477460014271,-197.872910446077,-196.873552312511,-195.874194178945,
-194.874836045379,-193.875477911813,-192.876119778247,-192.194274707092),
 .UNSPECIFIED.);
#335=B_SPLINE_CURVE_WITH_KNOTS('',3,(#16703,#16704,#16705,#16706,#16707,
#16708,#16709,#16710,#16711,#16712,#16713,#16714,#16715,#16716,#16717,#16718,
#16719,#16720,#16721,#16722,#16723,#16724),.UNSPECIFIED.,.F.,.F.,(4,3,3,
3,3,3,3,4),(188.938619885942,189.878045377549,190.877403511115,191.876761644681,
192.876119778247,193.875477911813,194.874836045379,195.221805193122),
 .UNSPECIFIED.);
#336=B_SPLINE_CURVE_WITH_KNOTS('',3,(#16729,#16730,#16731,#16732,#16733,
#16734,#16735,#16736,#16737,#16738,#16739,#16740,#16741,#16742,#16743,#16744,
#16745,#16746,#16747,#16748,#16749,#16750),.UNSPECIFIED.,.F.,.F.,(4,3,3,
3,3,3,3,4),(-204.760645321451,-203.869059247473,-202.869701113907,-201.870342980341,
-200.870984846775,-199.871626713209,-198.872268579643,-198.477460014271),
 .UNSPECIFIED.);
#337=B_SPLINE_CURVE_WITH_KNOTS('',3,(#16751,#16752,#16753,#16754,#16755,
#16756,#16757,#16758,#16759,#16760,#16761,#16762,#16763,#16764,#16765,#16766,
#16767,#16768,#16769,#16770,#16771,#16772),.UNSPECIFIED.,.F.,.F.,(4,3,3,
3,3,3,3,4),(195.221805193122,195.874194178945,196.873552312511,197.872910446077,
198.872268579643,199.871626713209,200.870984846776,201.504990500301),
 .UNSPECIFIED.);
#338=B_SPLINE_CURVE_WITH_KNOTS('',3,(#16777,#16778,#16779,#16780,#16781,
#16782,#16783,#16784,#16785,#16786,#16787,#16788,#16789,#16790,#16791,#16792,
#16793,#16794,#16795,#16796,#16797,#16798,#16799,#16800,#16801),
 .UNSPECIFIED.,.F.,.F.,(4,3,3,3,3,3,3,3,4),(-211.043830628631,-210.864566182436,
-209.86520804887,-208.865849915304,-207.866491781738,-206.867133648172,
-205.867775514606,-204.86841738104,-204.760645321451),.UNSPECIFIED.);
#339=B_SPLINE_CURVE_WITH_KNOTS('',3,(#16802,#16803,#16804,#16805,#16806,
#16807,#16808,#16809,#16810,#16811,#16812,#16813,#16814,#16815,#16816,#16817,
#16818,#16819,#16820,#16821,#16822,#16823),.UNSPECIFIED.,.F.,.F.,(4,3,3,
3,3,3,3,4),(201.504990500301,201.870342980342,202.869701113908,203.869059247474,
204.86841738104,205.867775514606,206.867133648172,207.788175807481),
 .UNSPECIFIED.);
#340=B_SPLINE_CURVE_WITH_KNOTS('',3,(#16828,#16829,#16830,#16831,#16832,
#16833,#16834,#16835,#16836,#16837,#16838,#16839,#16840,#16841,#16842,#16843,
#16844,#16845,#16846,#16847,#16848,#16849),.UNSPECIFIED.,.F.,.F.,(4,3,3,
3,3,3,3,4),(-217.32701593581,-216.860714983832,-215.861356850266,-214.8619987167,
-213.862640583134,-212.863282449568,-211.863924316002,-211.043830628631),
 .UNSPECIFIED.);
#341=B_SPLINE_CURVE_WITH_KNOTS('',3,(#16850,#16851,#16852,#16853,#16854,
#16855,#16856,#16857,#16858,#16859,#16860,#16861,#16862,#16863,#16864,#16865,
#16866,#16867,#16868,#16869,#16870,#16871,#16872,#16873,#16874),
 .UNSPECIFIED.,.F.,.F.,(4,3,3,3,3,3,3,3,4),(207.788175807481,207.866491781738,
208.865849915304,209.86520804887,210.864566182436,211.863924316002,212.863282449568,
213.862640583134,214.07136111466),.UNSPECIFIED.);
#342=B_SPLINE_CURVE_WITH_KNOTS('',3,(#16879,#16880,#16881,#16882,#16883,
#16884,#16885,#16886,#16887,#16888,#16889,#16890,#16891,#16892,#16893,#16894,
#16895,#16896,#16897,#16898,#16899,#16900),.UNSPECIFIED.,.F.,.F.,(4,3,3,
3,3,3,3,4),(-223.61020124299,-222.856863785228,-221.857505651662,-220.858147518096,
-219.85878938453,-218.859431250964,-217.860073117398,-217.32701593581),
 .UNSPECIFIED.);
#343=B_SPLINE_CURVE_WITH_KNOTS('',3,(#16901,#16902,#16903,#16904,#16905,
#16906,#16907,#16908,#16909,#16910,#16911,#16912,#16913,#16914,#16915,#16916,
#16917,#16918,#16919,#16920,#16921,#16922),.UNSPECIFIED.,.F.,.F.,(4,3,3,
3,3,3,3,4),(214.07136111466,214.8619987167,215.861356850266,216.860714983832,
217.860073117398,218.859431250964,219.85878938453,220.35454642184),
 .UNSPECIFIED.);
#344=B_SPLINE_CURVE_WITH_KNOTS('',3,(#16927,#16928,#16929,#16930,#16931,
#16932,#16933,#16934,#16935,#16936,#16937,#16938,#16939,#16940,#16941,#16942,
#16943,#16944,#16945,#16946,#16947,#16948,#16949,#16950,#16951),
 .UNSPECIFIED.,.F.,.F.,(4,3,3,3,3,3,3,3,4),(-229.893386550169,-229.852370720191,
-228.853012586625,-227.853654453059,-226.854296319493,-225.854938185927,
-224.85558005236,-223.856221918794,-223.61020124299),.UNSPECIFIED.);
#345=B_SPLINE_CURVE_WITH_KNOTS('',3,(#16952,#16953,#16954,#16955,#16956,
#16957,#16958,#16959,#16960,#16961,#16962,#16963,#16964,#16965,#16966,#16967,
#16968,#16969,#16970,#16971,#16972,#16973),.UNSPECIFIED.,.F.,.F.,(4,3,3,
3,3,3,3,4),(220.35454642184,220.858147518096,221.857505651663,222.856863785229,
223.856221918795,224.855580052361,225.854938185927,226.637731729019),
 .UNSPECIFIED.);
#346=B_SPLINE_CURVE_WITH_KNOTS('',3,(#16978,#16979,#16980,#16981,#16982,
#16983,#16984,#16985,#16986,#16987,#16988,#16989,#16990,#16991,#16992,#16993,
#16994,#16995,#16996,#16997,#16998,#16999),.UNSPECIFIED.,.F.,.F.,(4,3,3,
3,3,3,3,4),(-236.176571857349,-235.848519521587,-234.849161388021,-233.849803254455,
-232.850445120889,-231.851086987323,-230.851728853757,-229.893386550169),
 .UNSPECIFIED.);
#347=B_SPLINE_CURVE_WITH_KNOTS('',3,(#17000,#17001,#17002,#17003,#17004,
#17005,#17006,#17007,#17008,#17009,#17010,#17011,#17012,#17013,#17014,#17015,
#17016,#17017,#17018,#17019,#17020,#17021,#17022,#17023,#17024),
 .UNSPECIFIED.,.F.,.F.,(4,3,3,3,3,3,3,3,4),(226.637731729019,226.854296319493,
227.853654453059,228.853012586625,229.852370720191,230.851728853757,231.851086987323,
232.850445120889,232.920917036199),.UNSPECIFIED.);
#348=B_SPLINE_CURVE_WITH_KNOTS('',3,(#17029,#17030,#17031,#17032,#17033,
#17034,#17035,#17036,#17037,#17038,#17039,#17040,#17041,#17042,#17043,#17044,
#17045,#17046,#17047,#17048,#17049,#17050),.UNSPECIFIED.,.F.,.F.,(4,3,3,
3,3,3,3,4),(-242.459757164528,-241.844668322983,-240.845310189417,-239.845952055851,
-238.846593922285,-237.847235788719,-236.847877655153,-236.176571857349),
 .UNSPECIFIED.);
#349=B_SPLINE_CURVE_WITH_KNOTS('',3,(#17051,#17052,#17053,#17054,#17055,
#17056,#17057,#17058,#17059,#17060,#17061,#17062,#17063,#17064,#17065,#17066,
#17067,#17068,#17069,#17070,#17071,#17072),.UNSPECIFIED.,.F.,.F.,(4,3,3,
3,3,3,3,4),(232.920917036199,233.849803254455,234.849161388021,235.848519521587,
236.847877655153,237.847235788719,238.846593922285,239.204102343378),
 .UNSPECIFIED.);
#350=B_SPLINE_CURVE_WITH_KNOTS('',3,(#17077,#17078,#17079,#17080,#17081,
#17082,#17083,#17084,#17085,#17086,#17087,#17088,#17089,#17090,#17091,#17092,
#17093,#17094,#17095,#17096,#17097,#17098),.UNSPECIFIED.,.F.,.F.,(4,3,3,
3,3,3,3,4),(-248.742942471708,-247.84081712438,-246.841458990814,-245.842100857247,
-244.842742723681,-243.843384590115,-242.844026456549,-242.459757164528),
 .UNSPECIFIED.);
#351=B_SPLINE_CURVE_WITH_KNOTS('',3,(#17099,#17100,#17101,#17102,#17103,
#17104,#17105,#17106,#17107,#17108,#17109,#17110,#17111,#17112,#17113,#17114,
#17115,#17116,#17117,#17118,#17119,#17120),.UNSPECIFIED.,.F.,.F.,(4,3,3,
3,3,3,3,4),(239.204102343378,239.845952055851,240.845310189417,241.844668322983,
242.84402645655,243.843384590116,244.842742723682,245.487287650558),
 .UNSPECIFIED.);
#352=B_SPLINE_CURVE_WITH_KNOTS('',3,(#17125,#17126,#17127,#17128,#17129,
#17130,#17131,#17132,#17133,#17134,#17135,#17136,#17137,#17138,#17139,#17140,
#17141,#17142,#17143,#17144,#17145,#17146,#17147,#17148,#17149),
 .UNSPECIFIED.,.F.,.F.,(4,3,3,3,3,3,3,3,4),(-255.026127778888,-254.836324059342,
-253.836965925776,-252.83760779221,-251.838249658644,-250.838891525078,
-249.839533391512,-248.840175257946,-248.742942471708),.UNSPECIFIED.);
#353=B_SPLINE_CURVE_WITH_KNOTS('',3,(#17150,#17151,#17152,#17153,#17154,
#17155,#17156,#17157,#17158,#17159,#17160,#17161,#17162,#17163,#17164,#17165,
#17166,#17167,#17168,#17169,#17170,#17171),.UNSPECIFIED.,.F.,.F.,(4,3,3,
3,3,3,3,4),(245.487287650558,245.842100857248,246.841458990814,247.84081712438,
248.840175257946,249.839533391512,250.838891525078,251.770472957738),
 .UNSPECIFIED.);
#354=B_SPLINE_CURVE_WITH_KNOTS('',3,(#17176,#17177,#17178,#17179,#17180,
#17181,#17182,#17183,#17184,#17185,#17186,#17187,#17188,#17189,#17190,#17191,
#17192,#17193,#17194,#17195,#17196,#17197),.UNSPECIFIED.,.F.,.F.,(4,3,3,
3,3,3,3,4),(-261.309313086067,-260.832472860738,-259.833114727172,-258.833756593606,
-257.83439846004,-256.835040326474,-255.835682192908,-255.026127778888),
 .UNSPECIFIED.);
#355=B_SPLINE_CURVE_WITH_KNOTS('',3,(#17198,#17199,#17200,#17201,#17202,
#17203,#17204,#17205,#17206,#17207,#17208,#17209,#17210,#17211,#17212,#17213,
#17214,#17215,#17216,#17217,#17218,#17219,#17220,#17221,#17222),
 .UNSPECIFIED.,.F.,.F.,(4,3,3,3,3,3,3,3,4),(251.770472957738,251.838249658644,
252.83760779221,253.836965925776,254.836324059342,255.835682192908,256.835040326474,
257.83439846004,258.053658264917),.UNSPECIFIED.);
#356=B_SPLINE_CURVE_WITH_KNOTS('',3,(#17227,#17228,#17229,#17230,#17231,
#17232,#17233,#17234,#17235,#17236,#17237,#17238,#17239,#17240,#17241,#17242,
#17243,#17244,#17245,#17246,#17247,#17248),.UNSPECIFIED.,.F.,.F.,(4,3,3,
3,3,3,3,4),(-267.592498393247,-266.828621662134,-265.829263528568,-264.829905395002,
-263.830547261436,-262.83118912787,-261.831830994304,-261.309313086067),
 .UNSPECIFIED.);
#357=B_SPLINE_CURVE_WITH_KNOTS('',3,(#17249,#17250,#17251,#17252,#17253,
#17254,#17255,#17256,#17257,#17258,#17259,#17260,#17261,#17262,#17263,#17264,
#17265,#17266,#17267,#17268,#17269,#17270),.UNSPECIFIED.,.F.,.F.,(4,3,3,
3,3,3,3,4),(258.053658264917,258.833756593606,259.833114727172,260.832472860738,
261.831830994304,262.83118912787,263.830547261436,264.336843572097),
 .UNSPECIFIED.);
#358=B_SPLINE_CURVE_WITH_KNOTS('',3,(#17275,#17276,#17277,#17278,#17279,
#17280,#17281,#17282,#17283,#17284,#17285,#17286,#17287,#17288,#17289,#17290,
#17291,#17292,#17293,#17294,#17295,#17296,#17297,#17298,#17299),
 .UNSPECIFIED.,.F.,.F.,(4,3,3,3,3,3,3,3,4),(-273.875683700426,-273.824128597097,
-272.824770463531,-271.825412329965,-270.826054196399,-269.826696062833,
-268.827337929266,-267.8279797957,-267.592498393247),.UNSPECIFIED.);
#359=B_SPLINE_CURVE_WITH_KNOTS('',3,(#17300,#17301,#17302,#17303,#17304,
#17305,#17306,#17307,#17308,#17309,#17310,#17311,#17312,#17313,#17314,#17315,
#17316,#17317,#17318,#17319,#17320,#17321),.UNSPECIFIED.,.F.,.F.,(4,3,3,
3,3,3,3,4),(264.336843572097,264.829905395003,265.829263528569,266.828621662135,
267.827979795701,268.827337929267,269.826696062833,270.620028879276),
 .UNSPECIFIED.);
#360=B_SPLINE_CURVE_WITH_KNOTS('',3,(#17326,#17327,#17328,#17329,#17330,
#17331,#17332,#17333,#17334,#17335,#17336,#17337,#17338,#17339,#17340,#17341,
#17342,#17343,#17344,#17345,#17346,#17347),.UNSPECIFIED.,.F.,.F.,(4,3,3,
3,3,3,3,4),(-280.158869007606,-279.820277398493,-278.820919264927,-277.821561131361,
-276.822202997795,-275.822844864229,-274.823486730663,-273.875683700426),
 .UNSPECIFIED.);
#361=B_SPLINE_CURVE_WITH_KNOTS('',3,(#17348,#17349,#17350,#17351,#17352,
#17353,#17354,#17355,#17356,#17357,#17358,#17359,#17360,#17361,#17362,#17363,
#17364,#17365,#17366,#17367,#17368,#17369,#17370,#17371,#17372),
 .UNSPECIFIED.,.F.,.F.,(4,3,3,3,3,3,3,3,4),(270.620028879276,270.826054196399,
271.825412329965,272.824770463531,273.824128597097,274.823486730663,275.822844864229,
276.822202997795,276.903214186456),.UNSPECIFIED.);
#362=B_SPLINE_CURVE_WITH_KNOTS('',3,(#17377,#17378,#17379,#17380,#17381,
#17382,#17383,#17384,#17385,#17386,#17387,#17388,#17389,#17390,#17391,#17392,
#17393,#17394,#17395,#17396,#17397,#17398),.UNSPECIFIED.,.F.,.F.,(4,3,3,
3,3,3,3,4),(-286.442054314785,-285.816426199889,-284.817068066323,-283.817709932757,
-282.818351799191,-281.818993665625,-280.819635532059,-280.158869007606),
 .UNSPECIFIED.);
#363=B_SPLINE_CURVE_WITH_KNOTS('',3,(#17399,#17400,#17401,#17402,#17403,
#17404,#17405,#17406,#17407,#17408,#17409,#17410,#17411,#17412,#17413,#17414,
#17415,#17416,#17417,#17418,#17419,#17420),.UNSPECIFIED.,.F.,.F.,(4,3,3,
3,3,3,3,4),(276.903214186456,277.821561131361,278.820919264927,279.820277398493,
280.819635532059,281.818993665625,282.818351799191,283.186399493635),
 .UNSPECIFIED.);
#364=B_SPLINE_CURVE_WITH_KNOTS('',3,(#17425,#17426,#17427,#17428,#17429,
#17430,#17431,#17432,#17433,#17434,#17435,#17436,#17437,#17438,#17439,#17440,
#17441,#17442,#17443,#17444,#17445,#17446),.UNSPECIFIED.,.F.,.F.,(4,3,3,
3,3,3,3,4),(-292.725239621965,-291.812575001286,-290.81321686772,-289.813858734153,
-288.814500600587,-287.815142467021,-286.815784333455,-286.442054314785),
 .UNSPECIFIED.);
#365=B_SPLINE_CURVE_WITH_KNOTS('',3,(#17447,#17448,#17449,#17450,#17451,
#17452,#17453,#17454,#17455,#17456,#17457,#17458,#17459,#17460,#17461,#17462,
#17463,#17464,#17465,#17466,#17467,#17468),.UNSPECIFIED.,.F.,.F.,(4,3,3,
3,3,3,3,4),(283.186399493635,283.817709932757,284.817068066323,285.81642619989,
286.815784333456,287.815142467022,288.814500600588,289.469584800815),
 .UNSPECIFIED.);
#366=B_SPLINE_CURVE_WITH_KNOTS('',3,(#17473,#17474,#17475,#17476,#17477,
#17478,#17479,#17480,#17481,#17482,#17483,#17484,#17485,#17486,#17487,#17488,
#17489,#17490,#17491,#17492,#17493,#17494,#17495,#17496,#17497),
 .UNSPECIFIED.,.F.,.F.,(4,3,3,3,3,3,3,3,4),(-299.008424929145,-298.808081936248,
-297.808723802682,-296.809365669116,-295.81000753555,-294.810649401984,
-293.811291268418,-292.811933134852,-292.725239621965),.UNSPECIFIED.);
#367=B_SPLINE_CURVE_WITH_KNOTS('',3,(#17498,#17499,#17500,#17501,#17502,
#17503,#17504,#17505,#17506,#17507,#17508,#17509,#17510,#17511,#17512,#17513,
#17514,#17515,#17516,#17517,#17518,#17519),.UNSPECIFIED.,.F.,.F.,(4,3,3,
3,3,3,3,4),(289.469584800815,289.813858734154,290.81321686772,291.812575001286,
292.811933134852,293.811291268418,294.810649401984,295.752770107995),
 .UNSPECIFIED.);
#368=B_SPLINE_CURVE_WITH_KNOTS('',3,(#17524,#17525,#17526,#17527,#17528,
#17529,#17530,#17531,#17532,#17533,#17534,#17535,#17536,#17537,#17538,#17539,
#17540,#17541,#17542,#17543,#17544,#17545),.UNSPECIFIED.,.F.,.F.,(4,3,3,
3,3,3,3,4),(-305.291610236324,-304.804230737644,-303.804872604078,-302.805514470512,
-301.806156336946,-300.80679820338,-299.807440069814,-299.008424929145),
 .UNSPECIFIED.);
#369=B_SPLINE_CURVE_WITH_KNOTS('',3,(#17546,#17547,#17548,#17549,#17550,
#17551,#17552,#17553,#17554,#17555,#17556,#17557,#17558,#17559,#17560,#17561,
#17562,#17563,#17564,#17565,#17566,#17567,#17568,#17569,#17570),
 .UNSPECIFIED.,.F.,.F.,(4,3,3,3,3,3,3,3,4),(295.752770107995,295.81000753555,
296.809365669116,297.808723802682,298.808081936248,299.807440069814,300.80679820338,
301.806156336946,302.035955415174),.UNSPECIFIED.);
#370=B_SPLINE_CURVE_WITH_KNOTS('',3,(#17575,#17576,#17577,#17578,#17579,
#17580,#17581,#17582,#17583,#17584,#17585,#17586,#17587,#17588,#17589,#17590,
#17591,#17592,#17593,#17594,#17595,#17596),.UNSPECIFIED.,.F.,.F.,(4,3,3,
3,3,3,3,4),(-311.574795543504,-310.80037953904,-309.801021405475,-308.801663271908,
-307.802305138342,-306.802947004776,-305.80358887121,-305.291610236324),
 .UNSPECIFIED.);
#371=B_SPLINE_CURVE_WITH_KNOTS('',3,(#17597,#17598,#17599,#17600,#17601,
#17602,#17603,#17604,#17605,#17606,#17607,#17608,#17609,#17610,#17611,#17612,
#17613,#17614,#17615,#17616,#17617,#17618),.UNSPECIFIED.,.F.,.F.,(4,3,3,
3,3,3,3,4),(302.035955415174,302.805514470512,303.804872604078,304.804230737644,
305.80358887121,306.802947004777,307.802305138343,308.319140722354),
 .UNSPECIFIED.);
#372=B_SPLINE_CURVE_WITH_KNOTS('',3,(#17623,#17624,#17625,#17626,#17627,
#17628,#17629,#17630,#17631,#17632,#17633,#17634,#17635,#17636,#17637,#17638,
#17639,#17640,#17641,#17642,#17643,#17644,#17645,#17646,#17647),
 .UNSPECIFIED.,.F.,.F.,(4,3,3,3,3,3,3,3,4),(-317.857980850683,-317.795886474003,
-316.796528340437,-315.797170206871,-314.797812073305,-313.798453939739,
-312.799095806173,-311.799737672607,-311.574795543504),.UNSPECIFIED.);
#373=B_SPLINE_CURVE_WITH_KNOTS('',3,(#17648,#17649,#17650,#17651,#17652,
#17653,#17654,#17655,#17656,#17657,#17658,#17659,#17660,#17661,#17662,#17663,
#17664,#17665,#17666,#17667,#17668,#17669),.UNSPECIFIED.,.F.,.F.,(4,3,3,
3,3,3,3,4),(308.319140722354,308.801663271909,309.801021405475,310.800379539041,
311.799737672607,312.799095806173,313.798453939739,314.602326029533),
 .UNSPECIFIED.);
#374=B_SPLINE_CURVE_WITH_KNOTS('',3,(#17674,#17675,#17676,#17677,#17678,
#17679,#17680,#17681,#17682,#17683,#17684,#17685,#17686,#17687,#17688,#17689,
#17690,#17691,#17692,#17693,#17694,#17695),.UNSPECIFIED.,.F.,.F.,(4,3,3,
3,3,3,3,4),(-324.141166157863,-323.792035275399,-322.792677141833,-321.793319008267,
-320.793960874701,-319.794602741135,-318.795244607569,-317.857980850683),
 .UNSPECIFIED.);
#375=B_SPLINE_CURVE_WITH_KNOTS('',3,(#17696,#17697,#17698,#17699,#17700,
#17701,#17702,#17703,#17704,#17705,#17706,#17707,#17708,#17709,#17710,#17711,
#17712,#17713,#17714,#17715,#17716,#17717,#17718,#17719,#17720),
 .UNSPECIFIED.,.F.,.F.,(4,3,3,3,3,3,3,3,4),(314.602326029533,314.797812073305,
315.797170206871,316.796528340437,317.795886474003,318.795244607569,319.794602741135,
320.793960874701,320.885511336713),.UNSPECIFIED.);
#376=B_SPLINE_CURVE_WITH_KNOTS('',3,(#17725,#17726,#17727,#17728,#17729,
#17730,#17731,#17732,#17733,#17734,#17735,#17736,#17737,#17738,#17739,#17740,
#17741,#17742,#17743,#17744,#17745,#17746),.UNSPECIFIED.,.F.,.F.,(4,3,3,
3,3,3,3,4),(-330.424351465042,-329.788184076795,-328.788825943229,-327.789467809663,
-326.790109676097,-325.790751542531,-324.791393408965,-324.141166157863),
 .UNSPECIFIED.);
#377=B_SPLINE_CURVE_WITH_KNOTS('',3,(#17747,#17748,#17749,#17750,#17751,
#17752,#17753,#17754,#17755,#17756,#17757,#17758,#17759,#17760,#17761,#17762,
#17763,#17764,#17765,#17766,#17767,#17768),.UNSPECIFIED.,.F.,.F.,(4,3,3,
3,3,3,3,4),(320.885511336713,321.793319008267,322.792677141833,323.792035275399,
324.791393408965,325.790751542531,326.790109676097,327.168696643892),
 .UNSPECIFIED.);
#378=B_SPLINE_CURVE_WITH_KNOTS('',3,(#17773,#17774,#17775,#17776,#17777,
#17778,#17779,#17780,#17781,#17782,#17783,#17784,#17785,#17786,#17787,#17788,
#17789,#17790,#17791,#17792,#17793,#17794),.UNSPECIFIED.,.F.,.F.,(4,3,3,
3,3,3,3,4),(-336.707536772222,-335.784332878192,-334.784974744626,-333.78561661106,
-332.786258477494,-331.786900343927,-330.787542210361,-330.424351465042),
 .UNSPECIFIED.);
#379=B_SPLINE_CURVE_WITH_KNOTS('',3,(#17795,#17796,#17797,#17798,#17799,
#17800,#17801,#17802,#17803,#17804,#17805,#17806,#17807,#17808,#17809,#17810,
#17811,#17812,#17813,#17814,#17815,#17816),.UNSPECIFIED.,.F.,.F.,(4,3,3,
3,3,3,3,4),(327.168696643892,327.789467809663,328.78882594323,329.788184076796,
330.787542210362,331.786900343928,332.786258477494,333.451881951072),
 .UNSPECIFIED.);
#380=B_SPLINE_CURVE_WITH_KNOTS('',3,(#17821,#17822,#17823,#17824,#17825,
#17826,#17827,#17828,#17829,#17830,#17831,#17832,#17833,#17834,#17835,#17836,
#17837,#17838,#17839,#17840,#17841,#17842,#17843,#17844,#17845),
 .UNSPECIFIED.,.F.,.F.,(4,3,3,3,3,3,3,3,4),(-342.990722079402,-342.779839813154,
-341.780481679588,-340.781123546022,-339.781765412456,-338.78240727889,
-337.783049145324,-336.783691011758,-336.707536772222),.UNSPECIFIED.);
#381=B_SPLINE_CURVE_WITH_KNOTS('',3,(#17846,#17847,#17848,#17849,#17850,
#17851,#17852,#17853,#17854,#17855,#17856,#17857,#17858,#17859,#17860,#17861,
#17862,#17863,#17864,#17865,#17866,#17867),.UNSPECIFIED.,.F.,.F.,(4,3,3,
3,3,3,3,4),(333.451881951072,333.78561661106,334.784974744626,335.784332878192,
336.783691011758,337.783049145324,338.78240727889,339.735067258252),
 .UNSPECIFIED.);
#382=B_SPLINE_CURVE_WITH_KNOTS('',3,(#17872,#17873,#17874,#17875,#17876,
#17877,#17878,#17879,#17880,#17881,#17882,#17883,#17884,#17885,#17886,#17887,
#17888,#17889,#17890,#17891,#17892,#17893,#17894,#17895,#17896,#17897,#17898,
#17899,#17900,#17901,#17902,#17903,#17904,#17905),.UNSPECIFIED.,.F.,.F.,
(4,3,3,3,3,3,3,3,3,3,3,4),(-349.273907386581,-348.77598861455,-348.276309547767,
-347.776630480984,-347.276951414201,-346.777272347418,-346.277593280635,
-345.777914213852,-345.278235147069,-344.778556080286,-343.77919794672,
-342.990722079402),.UNSPECIFIED.);
#383=B_SPLINE_CURVE_WITH_KNOTS('',3,(#17906,#17907,#17908,#17909,#17910,
#17911,#17912,#17913,#17914,#17915,#17916,#17917,#17918,#17919,#17920,#17921,
#17922,#17923,#17924,#17925,#17926,#17927,#17928,#17929,#17930,#17931,#17932,
#17933),.UNSPECIFIED.,.F.,.F.,(4,3,3,3,3,3,3,3,3,4),(339.735067258252,339.781765412456,
340.781123546022,341.780481679588,342.779839813154,343.77919794672,344.778556080286,
345.278235147069,345.777914213852,346.018252565431),.UNSPECIFIED.);
#384=B_SPLINE_CURVE_WITH_KNOTS('',3,(#17938,#17939,#17940,#17941,#17942,
#17943,#17944,#17945,#17946,#17947,#17948,#17949,#17950,#17951,#17952,#17953,
#17954,#17955,#17956,#17957,#17958,#17959,#17960,#17961,#17962,#17963,#17964,
#17965,#17966,#17967,#17968,#17969,#17970,#17971,#17972,#17973,#17974,#17975,
#17976,#17977,#17978,#17979,#17980),.UNSPECIFIED.,.F.,.F.,(4,3,3,3,3,3,
3,3,3,3,3,3,3,3,4),(-355.557092693761,-355.27181648273,-354.772137415947,
-354.272458349164,-353.77277928238,-353.273100215597,-352.773421148814,
-352.273742082031,-351.774063015248,-351.274383948465,-350.774704881682,
-350.275025814899,-349.775346748116,-349.275667681333,-349.273907386581),
 .UNSPECIFIED.);
#385=B_SPLINE_CURVE_WITH_KNOTS('',3,(#17981,#17982,#17983,#17984,#17985,
#17986,#17987,#17988,#17989,#17990,#17991,#17992,#17993,#17994,#17995,#17996,
#17997,#17998,#17999,#18000,#18001,#18002,#18003,#18004,#18005,#18006,#18007,
#18008,#18009,#18010,#18011,#18012,#18013,#18014,#18015,#18016,#18017,#18018,
#18019,#18020,#18021,#18022,#18023),.UNSPECIFIED.,.F.,.F.,(4,3,3,3,3,3,
3,3,3,3,3,3,3,3,4),(346.018252565431,346.277593280635,346.777272347418,
347.276951414201,347.776630480984,348.276309547767,348.77598861455,349.275667681334,
349.775346748116,350.2750258149,350.774704881683,351.274383948466,351.774063015249,
352.273742082032,352.301437872611),.UNSPECIFIED.);
#386=B_SPLINE_CURVE_WITH_KNOTS('',3,(#18028,#18029,#18030,#18031,#18032,
#18033,#18034,#18035,#18036,#18037,#18038,#18039,#18040,#18041,#18042,#18043,
#18044,#18045,#18046,#18047,#18048,#18049,#18050,#18051,#18052,#18053,#18054,
#18055,#18056,#18057,#18058,#18059,#18060,#18061,#18062,#18063,#18064,#18065,
#18066,#18067,#18068,#18069,#18070),.UNSPECIFIED.,.F.,.F.,(4,3,3,3,3,3,
3,3,3,3,3,3,3,3,4),(-361.84027800094,-361.767644350909,-361.267965284126,
-360.768286217343,-360.26860715056,-359.768928083777,-359.269249016994,
-358.769569950211,-358.269890883428,-357.770211816645,-357.270532749862,
-356.770853683079,-356.271174616296,-355.771495549513,-355.557092693761),
 .UNSPECIFIED.);
#387=B_SPLINE_CURVE_WITH_KNOTS('',3,(#18071,#18072,#18073,#18074,#18075,
#18076,#18077,#18078,#18079,#18080,#18081,#18082,#18083,#18084,#18085,#18086,
#18087,#18088,#18089,#18090,#18091,#18092,#18093,#18094,#18095,#18096,#18097,
#18098,#18099,#18100,#18101,#18102,#18103,#18104,#18105,#18106,#18107,#18108,
#18109,#18110),.UNSPECIFIED.,.F.,.F.,(4,3,3,3,3,3,3,3,3,3,3,3,3,4),(352.301437872611,
352.773421148815,353.273100215598,353.772779282381,354.272458349164,354.772137415947,
355.27181648273,355.771495549513,356.271174616296,356.770853683079,357.270532749862,
357.770211816645,358.269890883428,358.58462317979),.UNSPECIFIED.);
#388=B_SPLINE_CURVE_WITH_KNOTS('',3,(#18115,#18116,#18117,#18118,#18119,
#18120,#18121,#18122,#18123,#18124,#18125,#18126,#18127,#18128,#18129,#18130,
#18131,#18132,#18133,#18134,#18135,#18136,#18137,#18138,#18139,#18140,#18141,
#18142,#18143,#18144,#18145,#18146,#18147,#18148,#18149,#18150,#18151,#18152,
#18153,#18154),.UNSPECIFIED.,.F.,.F.,(4,3,3,3,3,3,3,3,3,3,3,3,3,4),(-368.12346330812,
-367.763793152305,-367.264114085522,-366.764435018739,-366.264755951956,
-365.765076885173,-365.26539781839,-364.765718751607,-364.266039684824,
-363.766360618041,-363.266681551258,-362.767002484475,-362.267323417692,
-361.84027800094),.UNSPECIFIED.);
#389=B_SPLINE_CURVE_WITH_KNOTS('',3,(#18155,#18156,#18157,#18158,#18159,
#18160,#18161,#18162,#18163,#18164,#18165,#18166,#18167,#18168,#18169,#18170,
#18171,#18172,#18173,#18174,#18175,#18176,#18177,#18178,#18179,#18180,#18181,
#18182,#18183,#18184,#18185,#18186,#18187,#18188,#18189,#18190,#18191,#18192,
#18193,#18194,#18195,#18196,#18197),.UNSPECIFIED.,.F.,.F.,(4,3,3,3,3,3,
3,3,3,3,3,3,3,3,4),(358.58462317979,358.769569950211,359.269249016994,359.768928083777,
360.26860715056,360.768286217343,361.267965284126,361.767644350909,362.267323417692,
362.767002484475,363.266681551258,363.766360618041,364.266039684824,364.765718751607,
364.86780848697),.UNSPECIFIED.);
#390=B_SPLINE_CURVE_WITH_KNOTS('',3,(#18202,#18203,#18204,#18205,#18206,
#18207,#18208,#18209,#18210,#18211,#18212,#18213,#18214,#18215,#18216,#18217,
#18218,#18219,#18220,#18221,#18222,#18223,#18224,#18225,#18226,#18227,#18228,
#18229,#18230,#18231,#18232,#18233,#18234,#18235,#18236,#18237,#18238,#18239,
#18240,#18241,#18242,#18243,#18244),.UNSPECIFIED.,.F.,.F.,(4,3,3,3,3,3,
3,3,3,3,3,3,3,3,4),(-374.406648615299,-374.259621020484,-373.759941953701,
-373.260262886918,-372.760583820135,-372.260904753352,-371.761225686569,
-371.261546619786,-370.761867553003,-370.26218848622,-369.762509419437,
-369.262830352654,-368.763151285871,-368.263472219088,-368.12346330812),
 .UNSPECIFIED.);
#391=B_SPLINE_CURVE_WITH_KNOTS('',3,(#18245,#18246,#18247,#18248,#18249,
#18250,#18251,#18252,#18253,#18254,#18255,#18256,#18257,#18258,#18259,#18260,
#18261,#18262,#18263,#18264,#18265,#18266,#18267,#18268,#18269,#18270,#18271,
#18272,#18273,#18274,#18275,#18276,#18277,#18278,#18279,#18280,#18281,#18282,
#18283,#18284),.UNSPECIFIED.,.F.,.F.,(4,3,3,3,3,3,3,3,3,3,3,3,3,4),(364.86780848697,
365.26539781839,365.765076885173,366.264755951956,366.764435018739,367.264114085522,
367.763793152305,368.263472219088,368.763151285871,369.262830352654,369.762509419437,
370.26218848622,370.761867553004,371.150993794149),.UNSPECIFIED.);
#392=B_SPLINE_CURVE_WITH_KNOTS('',3,(#18289,#18290,#18291,#18292,#18293,
#18294,#18295,#18296,#18297,#18298,#18299,#18300,#18301,#18302,#18303,#18304,
#18305,#18306,#18307,#18308,#18309,#18310,#18311,#18312,#18313,#18314,#18315,
#18316,#18317,#18318,#18319,#18320,#18321,#18322,#18323,#18324,#18325,#18326,
#18327,#18328),.UNSPECIFIED.,.F.,.F.,(4,3,3,3,3,3,3,3,3,3,3,3,3,4),(-380.689833922479,
-380.255769821881,-379.756090755098,-379.256411688315,-378.756732621532,
-378.257053554749,-377.757374487966,-377.257695421183,-376.7580163544,-376.258337287616,
-375.758658220834,-375.25897915405,-374.759300087267,-374.406648615299),
 .UNSPECIFIED.);
#393=B_SPLINE_CURVE_WITH_KNOTS('',3,(#18329,#18330,#18331,#18332,#18333,
#18334,#18335,#18336,#18337,#18338,#18339,#18340,#18341,#18342,#18343,#18344,
#18345,#18346,#18347,#18348,#18349,#18350,#18351,#18352,#18353,#18354,#18355,
#18356,#18357,#18358,#18359,#18360,#18361,#18362,#18363,#18364,#18365,#18366,
#18367,#18368,#18369,#18370,#18371),.UNSPECIFIED.,.F.,.F.,(4,3,3,3,3,3,
3,3,3,3,3,3,3,3,4),(371.150993794149,371.261546619787,371.76122568657,372.260904753353,
372.760583820136,373.260262886919,373.759941953702,374.259621020485,374.759300087268,
375.258979154051,375.758658220834,376.258337287617,376.7580163544,377.257695421183,
377.434179101329),.UNSPECIFIED.);
#394=B_SPLINE_CURVE_WITH_KNOTS('',3,(#18376,#18377,#18378,#18379,#18380,
#18381,#18382,#18383,#18384,#18385,#18386,#18387,#18388,#18389,#18390,#18391,
#18392,#18393,#18394,#18395,#18396,#18397,#18398,#18399,#18400,#18401,#18402,
#18403,#18404,#18405,#18406,#18407,#18408,#18409,#18410,#18411,#18412,#18413,
#18414,#18415,#18416,#18417,#18418),.UNSPECIFIED.,.F.,.F.,(4,3,3,3,3,3,
3,3,3,3,3,3,3,3,4),(-386.973019229658,-386.75159769006,-386.251918623277,
-385.752239556494,-385.252560489711,-384.752881422928,-384.253202356145,
-383.753523289362,-383.253844222579,-382.754165155796,-382.254486089013,
-381.75480702223,-381.255127955447,-380.755448888664,-380.689833922479),
 .UNSPECIFIED.);
#395=B_SPLINE_CURVE_WITH_KNOTS('',3,(#18419,#18420,#18421,#18422,#18423,
#18424,#18425,#18426,#18427,#18428,#18429,#18430,#18431,#18432,#18433,#18434,
#18435,#18436,#18437,#18438,#18439,#18440,#18441,#18442,#18443,#18444,#18445,
#18446,#18447,#18448,#18449,#18450,#18451,#18452,#18453,#18454,#18455,#18456,
#18457,#18458),.UNSPECIFIED.,.F.,.F.,(4,3,3,3,3,3,3,3,3,3,3,3,3,4),(377.434179101329,
377.757374487966,378.257053554749,378.756732621532,379.256411688315,379.756090755098,
380.255769821881,380.755448888664,381.255127955447,381.75480702223,382.254486089013,
382.754165155796,383.253844222579,383.717364408508),.UNSPECIFIED.);
#396=B_SPLINE_CURVE_WITH_KNOTS('',3,(#18463,#18464,#18465,#18466,#18467,
#18468,#18469,#18470,#18471,#18472,#18473,#18474,#18475,#18476,#18477,#18478,
#18479,#18480,#18481,#18482,#18483,#18484,#18485,#18486,#18487,#18488,#18489,
#18490,#18491,#18492,#18493,#18494,#18495,#18496,#18497,#18498,#18499,#18500,
#18501,#18502,#18503,#18504,#18505),.UNSPECIFIED.,.F.,.F.,(4,3,3,3,3,3,
3,3,3,3,3,3,3,3,4),(-393.256204536838,-393.247425558239,-392.747746491456,
-392.248067424673,-391.74838835789,-391.248709291107,-390.749030224324,
-390.249351157541,-389.749672090758,-389.249993023975,-388.750313957192,
-388.250634890409,-387.750955823626,-387.251276756843,-386.973019229658),
 .UNSPECIFIED.);
#397=B_SPLINE_CURVE_WITH_KNOTS('',3,(#18506,#18507,#18508,#18509,#18510,
#18511,#18512,#18513,#18514,#18515,#18516,#18517,#18518,#18519,#18520,#18521,
#18522,#18523,#18524,#18525,#18526,#18527,#18528,#18529,#18530,#18531,#18532,
#18533,#18534,#18535,#18536,#18537,#18538,#18539,#18540,#18541,#18542,#18543,
#18544,#18545,#18546,#18547,#18548),.UNSPECIFIED.,.F.,.F.,(4,3,3,3,3,3,
3,3,3,3,3,3,3,3,4),(383.717364408508,383.753523289362,384.253202356145,
384.752881422928,385.252560489711,385.752239556494,386.251918623277,386.75159769006,
387.251276756843,387.750955823626,388.250634890409,388.750313957192,389.249993023975,
389.749672090758,390.000549715688),.UNSPECIFIED.);
#398=B_SPLINE_CURVE_WITH_KNOTS('',3,(#18554,#18555,#18556,#18557),
 .UNSPECIFIED.,.F.,.F.,(4,4),(405.265452313083,405.755527026166),
 .UNSPECIFIED.);
#399=B_SPLINE_CURVE_WITH_KNOTS('',3,(#18563,#18564,#18565,#18566,#18567,
#18568,#18569,#18570,#18571,#18572,#18573,#18574,#18575,#18576,#18577,#18578,
#18579),.UNSPECIFIED.,.F.,.F.,(4,1,1,1,1,1,1,1,1,1,1,1,1,1,4),(398.982267005903,
399.260524533088,399.760203599871,400.259882666654,400.759561733437,401.25924080022,
401.758919867003,402.258598933787,402.75827800057,403.257957067353,403.757636134136,
404.257315200919,404.756994267702,405.256673334485,405.265452313083),
 .UNSPECIFIED.);
#400=B_SPLINE_CURVE_WITH_KNOTS('',3,(#18582,#18583,#18584,#18585,#18586,
#18587,#18588,#18589,#18590,#18591,#18592,#18593,#18594),.UNSPECIFIED.,
 .F.,.F.,(4,1,1,1,1,1,1,1,1,1,4),(398.982267005904,399.231068447758,399.730747514541,
400.230426581324,400.730105648107,401.22978471489,401.729463781673,402.229142848456,
402.728821915239,403.228500982022,403.728180048805),.UNSPECIFIED.);
#401=B_SPLINE_CURVE_WITH_KNOTS('',3,(#18599,#18600,#18601,#18602,#18603,
#18604,#18605,#18606,#18607,#18608,#18609,#18610,#18611,#18612,#18613,#18614,
#18615),.UNSPECIFIED.,.F.,.F.,(4,1,1,1,1,1,1,1,1,1,1,1,1,1,4),(392.699081698724,
392.764696664909,393.264375731692,393.764054798475,394.263733865258,394.763412932041,
395.263091998824,395.762771065607,396.26245013239,396.762129199173,397.261808265956,
397.761487332739,398.261166399522,398.760845466305,398.982267005903),
 .UNSPECIFIED.);
#402=B_SPLINE_CURVE_WITH_KNOTS('',3,(#18616,#18617,#18618,#18619,#18620,
#18621,#18622,#18623,#18624,#18625,#18626,#18627,#18628,#18629,#18630,#18631,
#18632),.UNSPECIFIED.,.F.,.F.,(4,1,1,1,1,1,1,1,1,1,1,1,1,1,4),(392.699081698724,
392.735240579579,393.234919646362,393.734598713145,394.234277779928,394.733956846711,
395.233635913494,395.733314980277,396.23299404706,396.732673113843,397.232352180626,
397.732031247409,398.231710314192,398.731389380975,398.982267005904),
 .UNSPECIFIED.);
#403=B_SPLINE_CURVE_WITH_KNOTS('',3,(#18637,#18638,#18639,#18640,#18641,
#18642,#18643,#18644,#18645,#18646,#18647,#18648,#18649,#18650,#18651,#18652),
 .UNSPECIFIED.,.F.,.F.,(4,1,1,1,1,1,1,1,1,1,1,1,1,4),(386.415896391544,
386.768547863513,387.268226930296,387.767905997079,388.267585063862,388.767264130645,
389.266943197428,389.766622264211,390.266301330994,390.765980397777,391.26565946456,
391.765338531343,392.265017598126,392.699081698724),.UNSPECIFIED.);
#404=B_SPLINE_CURVE_WITH_KNOTS('',3,(#18653,#18654,#18655,#18656,#18657,
#18658,#18659,#18660,#18661,#18662,#18663,#18664,#18665,#18666,#18667,#18668),
 .UNSPECIFIED.,.F.,.F.,(4,1,1,1,1,1,1,1,1,1,1,1,1,4),(386.415896391545,
386.739091778183,387.238770844966,387.738449911749,388.238128978532,388.737808045315,
389.237487112098,389.737166178881,390.236845245664,390.736524312447,391.23620337923,
391.735882446013,392.235561512796,392.699081698724),.UNSPECIFIED.);
#405=B_SPLINE_CURVE_WITH_KNOTS('',3,(#18673,#18674,#18675,#18676,#18677,
#18678,#18679,#18680,#18681,#18682,#18683,#18684,#18685,#18686,#18687,#18688,
#18689),.UNSPECIFIED.,.F.,.F.,(4,1,1,1,1,1,1,1,1,1,1,1,1,1,4),(380.132711084365,
380.272719995333,380.772399062117,381.2720781289,381.771757195683,382.271436262466,
382.771115329249,383.270794396032,383.770473462815,384.270152529598,384.769831596381,
385.269510663164,385.769189729947,386.26886879673,386.415896391544),
 .UNSPECIFIED.);
#406=B_SPLINE_CURVE_WITH_KNOTS('',3,(#18690,#18691,#18692,#18693,#18694,
#18695,#18696,#18697,#18698,#18699,#18700,#18701,#18702,#18703,#18704,#18705,
#18706),.UNSPECIFIED.,.F.,.F.,(4,1,1,1,1,1,1,1,1,1,1,1,1,1,4),(380.132711084365,
380.243263910003,380.742942976786,381.242622043569,381.742301110352,382.241980177135,
382.741659243918,383.241338310702,383.741017377485,384.240696444268,384.740375511051,
385.240054577834,385.739733644617,386.2394127114,386.415896391545),
 .UNSPECIFIED.);
#407=B_SPLINE_CURVE_WITH_KNOTS('',3,(#18711,#18712,#18713,#18714,#18715,
#18716,#18717,#18718,#18719,#18720,#18721,#18722,#18723,#18724,#18725,#18726),
 .UNSPECIFIED.,.F.,.F.,(4,1,1,1,1,1,1,1,1,1,1,1,1,4),(373.849525777185,
374.276571193937,374.77625026072,375.275929327503,375.775608394286,376.275287461069,
376.774966527852,377.274645594635,377.774324661418,378.274003728201,378.773682794984,
379.273361861767,379.77304092855,380.132711084365),.UNSPECIFIED.);
#408=B_SPLINE_CURVE_WITH_KNOTS('',3,(#18727,#18728,#18729,#18730,#18731,
#18732,#18733,#18734,#18735,#18736,#18737,#18738,#18739,#18740,#18741,#18742),
 .UNSPECIFIED.,.F.,.F.,(4,1,1,1,1,1,1,1,1,1,1,1,1,4),(373.849525777185,
374.247115108607,374.74679417539,375.246473242173,375.746152308956,376.245831375739,
376.745510442522,377.245189509305,377.744868576088,378.244547642871,378.744226709654,
379.243905776437,379.74358484322,380.132711084365),.UNSPECIFIED.);
#409=B_SPLINE_CURVE_WITH_KNOTS('',3,(#18747,#18748,#18749,#18750,#18751,
#18752,#18753,#18754,#18755,#18756,#18757,#18758,#18759,#18760,#18761,#18762,
#18763),.UNSPECIFIED.,.F.,.F.,(4,1,1,1,1,1,1,1,1,1,1,1,1,1,4),(367.566340470006,
367.780743325758,368.280422392541,368.780101459324,369.279780526107,369.77945959289,
370.279138659673,370.778817726456,371.278496793239,371.778175860022,372.277854926805,
372.777533993588,373.277213060371,373.776892127154,373.849525777185),
 .UNSPECIFIED.);
#410=B_SPLINE_CURVE_WITH_KNOTS('',3,(#18764,#18765,#18766,#18767,#18768,
#18769,#18770,#18771,#18772,#18773,#18774,#18775,#18776,#18777,#18778,#18779,
#18780),.UNSPECIFIED.,.F.,.F.,(4,1,1,1,1,1,1,1,1,1,1,1,1,1,4),(367.566340470006,
367.751287240428,368.250966307211,368.750645373994,369.250324440777,369.75000350756,
370.249682574343,370.749361641126,371.249040707909,371.748719774692,372.248398841475,
372.748077908258,373.247756975041,373.747436041824,373.849525777185),
 .UNSPECIFIED.);
#411=B_SPLINE_CURVE_WITH_KNOTS('',3,(#18785,#18786,#18787,#18788,#18789,
#18790,#18791,#18792,#18793,#18794,#18795,#18796,#18797,#18798,#18799,#18800,
#18801),.UNSPECIFIED.,.F.,.F.,(4,1,1,1,1,1,1,1,1,1,1,1,1,1,4),(361.283155162826,
361.284915457579,361.784594524362,362.284273591145,362.783952657928,363.283631724711,
363.783310791494,364.282989858277,364.78266892506,365.282347991843,365.782027058626,
366.281706125409,366.781385192192,367.281064258975,367.566340470006),
 .UNSPECIFIED.);
#412=B_SPLINE_CURVE_WITH_KNOTS('',3,(#18802,#18803,#18804,#18805,#18806,
#18807,#18808,#18809,#18810,#18811,#18812,#18813,#18814,#18815,#18816,#18817),
 .UNSPECIFIED.,.F.,.F.,(4,1,1,1,1,1,1,1,1,1,1,1,1,4),(361.283155162826,
361.755138439031,362.254817505815,362.754496572598,363.254175639381,363.753854706164,
364.253533772947,364.75321283973,365.252891906513,365.752570973296,366.252250040079,
366.751929106862,367.251608173645,367.566340470006),.UNSPECIFIED.);
#413=B_SPLINE_CURVE_WITH_KNOTS('',3,(#18822,#18823,#18824,#18825,#18826,
#18827,#18828,#18829,#18830,#18831,#18832,#18833,#18834,#18835),
 .UNSPECIFIED.,.F.,.F.,(4,1,1,1,1,1,1,1,1,1,1,4),(354.999969855646,355.788445722965,
356.787803856531,357.287482923314,357.787161990097,358.28684105688,358.786520123663,
359.286199190446,359.78587825723,360.285557324013,360.785236390796,361.283155162826),
 .UNSPECIFIED.);
#414=B_SPLINE_CURVE_WITH_KNOTS('',3,(#18836,#18837,#18838,#18839,#18840,
#18841,#18842,#18843,#18844,#18845,#18846,#18847,#18848,#18849,#18850,#18851,
#18852),.UNSPECIFIED.,.F.,.F.,(4,1,1,1,1,1,1,1,1,1,1,1,1,1,4),(354.999969855647,
355.259310570852,355.758989637635,356.258668704418,356.758347771201,357.258026837984,
357.757705904767,358.25738497155,358.757064038333,359.256743105116,359.756422171899,
360.256101238682,360.755780305465,361.255459372248,361.283155162826),
 .UNSPECIFIED.);
#415=B_SPLINE_CURVE_WITH_KNOTS('',3,(#18857,#18858,#18859,#18860,#18861,
#18862,#18863,#18864,#18865,#18866,#18867),.UNSPECIFIED.,.F.,.F.,(4,1,1,
1,1,1,1,1,4),(348.716784548467,348.792938788003,349.792296921569,350.791655055135,
351.791013188701,352.790371322267,353.789729455833,354.789087589399,354.999969855646),
 .UNSPECIFIED.);
#416=B_SPLINE_CURVE_WITH_KNOTS('',3,(#18868,#18869,#18870,#18871,#18872,
#18873,#18874,#18875,#18876,#18877,#18878,#18879),.UNSPECIFIED.,.F.,.F.,
(4,1,1,1,1,1,1,1,1,4),(348.716784548467,348.763482702673,349.762840836239,
350.762198969805,351.761557103371,352.760915236937,353.760273370503,354.259952437286,
354.759631504069,354.999969855647),.UNSPECIFIED.);
#417=B_SPLINE_CURVE_WITH_KNOTS('',3,(#18884,#18885,#18886,#18887,#18888,
#18889,#18890,#18891,#18892,#18893),.UNSPECIFIED.,.F.,.F.,(4,1,1,1,1,1,
1,4),(342.433599241287,342.796789986607,343.796148120173,344.795506253739,
345.794864387305,346.794222520871,347.793580654437,348.716784548467),
 .UNSPECIFIED.);
#418=B_SPLINE_CURVE_WITH_KNOTS('',3,(#18894,#18895,#18896,#18897,#18898,
#18899,#18900,#18901,#18902,#18903),.UNSPECIFIED.,.F.,.F.,(4,1,1,1,1,1,
1,4),(342.433599241288,342.767333901277,343.766692034843,344.766050168409,
345.765408301975,346.764766435541,347.764124569107,348.716784548467),
 .UNSPECIFIED.);
#419=B_SPLINE_CURVE_WITH_KNOTS('',3,(#18908,#18909,#18910,#18911,#18912,
#18913,#18914,#18915,#18916,#18917),.UNSPECIFIED.,.F.,.F.,(4,1,1,1,1,1,
1,4),(336.150413934108,336.80064118521,337.799999318776,338.799357452343,
339.798715585909,340.798073719475,341.797431853041,342.433599241287),
 .UNSPECIFIED.);
#420=B_SPLINE_CURVE_WITH_KNOTS('',3,(#18918,#18919,#18920,#18921,#18922,
#18923,#18924,#18925,#18926,#18927),.UNSPECIFIED.,.F.,.F.,(4,1,1,1,1,1,
1,4),(336.150413934108,336.77118509988,337.770543233446,338.769901367012,
339.769259500578,340.768617634145,341.767975767711,342.433599241288),
 .UNSPECIFIED.);
#421=B_SPLINE_CURVE_WITH_KNOTS('',3,(#18932,#18933,#18934,#18935,#18936,
#18937,#18938,#18939,#18940,#18941),.UNSPECIFIED.,.F.,.F.,(4,1,1,1,1,1,
1,4),(329.867228626928,330.804492383814,331.80385051738,332.803208650946,
333.802566784512,334.801924918078,335.801283051644,336.150413934108),
 .UNSPECIFIED.);
#422=B_SPLINE_CURVE_WITH_KNOTS('',3,(#18942,#18943,#18944,#18945,#18946,
#18947,#18948,#18949,#18950,#18951),.UNSPECIFIED.,.F.,.F.,(4,1,1,1,1,1,
1,4),(329.867228626928,330.775036298484,331.77439443205,332.773752565616,
333.773110699182,334.772468832748,335.771826966314,336.150413934108),
 .UNSPECIFIED.);
#423=B_SPLINE_CURVE_WITH_KNOTS('',3,(#18956,#18957,#18958,#18959,#18960,
#18961,#18962,#18963,#18964,#18965,#18966),.UNSPECIFIED.,.F.,.F.,(4,1,1,
1,1,1,1,1,4),(323.584043319749,323.808985448852,324.808343582418,325.807701715984,
326.80705984955,327.806417983116,328.805776116682,329.805134250248,329.867228626928),
 .UNSPECIFIED.);
#424=B_SPLINE_CURVE_WITH_KNOTS('',3,(#18967,#18968,#18969,#18970,#18971,
#18972,#18973,#18974,#18975,#18976,#18977),.UNSPECIFIED.,.F.,.F.,(4,1,1,
1,1,1,1,1,4),(323.584043319749,323.779529363522,324.778887497088,325.778245630654,
326.77760376422,327.776961897786,328.776320031352,329.775678164918,329.867228626928),
 .UNSPECIFIED.);
#425=B_SPLINE_CURVE_WITH_KNOTS('',3,(#18982,#18983,#18984,#18985,#18986,
#18987,#18988,#18989,#18990,#18991),.UNSPECIFIED.,.F.,.F.,(4,1,1,1,1,1,
1,4),(317.300858012569,317.812836647456,318.812194781022,319.811552914588,
320.810911048154,321.81026918172,322.809627315286,323.584043319749),
 .UNSPECIFIED.);
#426=B_SPLINE_CURVE_WITH_KNOTS('',3,(#18992,#18993,#18994,#18995,#18996,
#18997,#18998,#18999,#19000,#19001),.UNSPECIFIED.,.F.,.F.,(4,1,1,1,1,1,
1,4),(317.300858012569,317.783380562125,318.782738695691,319.782096829258,
320.781454962824,321.78081309639,322.780171229956,323.584043319749),
 .UNSPECIFIED.);
#427=B_SPLINE_CURVE_WITH_KNOTS('',3,(#19006,#19007,#19008,#19009,#19010,
#19011,#19012,#19013,#19014,#19015),.UNSPECIFIED.,.F.,.F.,(4,1,1,1,1,1,
1,4),(311.017672705389,311.816687846059,312.816045979625,313.815404113191,
314.814762246757,315.814120380323,316.81347851389,317.300858012569),
 .UNSPECIFIED.);
#428=B_SPLINE_CURVE_WITH_KNOTS('',3,(#19016,#19017,#19018,#19019,#19020,
#19021,#19022,#19023,#19024,#19025),.UNSPECIFIED.,.F.,.F.,(4,1,1,1,1,1,
1,4),(311.01767270539,311.787231760729,312.786589894295,313.785948027861,
314.785306161427,315.784664294993,316.784022428559,317.300858012569),
 .UNSPECIFIED.);
#429=B_SPLINE_CURVE_WITH_KNOTS('',3,(#19030,#19031,#19032,#19033,#19034,
#19035,#19036,#19037,#19038,#19039,#19040),.UNSPECIFIED.,.F.,.F.,(4,1,1,
1,1,1,1,1,4),(304.73448739821,304.821180911097,305.820539044663,306.819897178229,
307.819255311795,308.818613445361,309.817971578927,310.817329712493,311.017672705389),
 .UNSPECIFIED.);
#430=B_SPLINE_CURVE_WITH_KNOTS('',3,(#19041,#19042,#19043,#19044,#19045,
#19046,#19047,#19048,#19049,#19050,#19051),.UNSPECIFIED.,.F.,.F.,(4,1,1,
1,1,1,1,1,4),(304.73448739821,304.791724825767,305.791082959333,306.790441092899,
307.789799226465,308.789157360031,309.788515493597,310.787873627163,311.01767270539),
 .UNSPECIFIED.);
#431=B_SPLINE_CURVE_WITH_KNOTS('',3,(#19056,#19057,#19058,#19059,#19060,
#19061,#19062,#19063,#19064,#19065),.UNSPECIFIED.,.F.,.F.,(4,1,1,1,1,1,
1,4),(298.45130209103,298.825032109701,299.824390243267,300.823748376833,
301.823106510399,302.822464643965,303.821822777531,304.73448739821),
 .UNSPECIFIED.);
#432=B_SPLINE_CURVE_WITH_KNOTS('',3,(#19066,#19067,#19068,#19069,#19070,
#19071,#19072,#19073,#19074,#19075),.UNSPECIFIED.,.F.,.F.,(4,1,1,1,1,1,
1,4),(298.451302091031,298.795576024371,299.794934157937,300.794292291503,
301.793650425069,302.793008558635,303.792366692201,304.73448739821),
 .UNSPECIFIED.);
#433=B_SPLINE_CURVE_WITH_KNOTS('',3,(#19080,#19081,#19082,#19083,#19084,
#19085,#19086,#19087,#19088,#19089),.UNSPECIFIED.,.F.,.F.,(4,1,1,1,1,1,
1,4),(292.168116783851,292.828883308304,293.82824144187,294.827599575437,
295.826957709003,296.826315842569,297.825673976135,298.45130209103),
 .UNSPECIFIED.);
#434=B_SPLINE_CURVE_WITH_KNOTS('',3,(#19090,#19091,#19092,#19093,#19094,
#19095,#19096,#19097,#19098,#19099),.UNSPECIFIED.,.F.,.F.,(4,1,1,1,1,1,
1,4),(292.168116783851,292.799427222974,293.79878535654,294.798143490106,
295.797501623672,296.796859757238,297.796217890804,298.451302091031),
 .UNSPECIFIED.);
#435=B_SPLINE_CURVE_WITH_KNOTS('',3,(#19104,#19105,#19106,#19107,#19108,
#19109,#19110,#19111,#19112,#19113),.UNSPECIFIED.,.F.,.F.,(4,1,1,1,1,1,
1,4),(285.884931476671,286.832734506908,287.832092640474,288.83145077404,
289.830808907606,290.830167041172,291.829525174738,292.168116783851),
 .UNSPECIFIED.);
#436=B_SPLINE_CURVE_WITH_KNOTS('',3,(#19114,#19115,#19116,#19117,#19118,
#19119,#19120,#19121,#19122,#19123),.UNSPECIFIED.,.F.,.F.,(4,1,1,1,1,1,
1,4),(285.884931476672,286.803278421578,287.802636555144,288.80199468871,
289.801352822276,290.800710955842,291.800069089408,292.168116783851),
 .UNSPECIFIED.);
#437=B_SPLINE_CURVE_WITH_KNOTS('',3,(#19128,#19129,#19130,#19131,#19132,
#19133,#19134,#19135,#19136,#19137,#19138),.UNSPECIFIED.,.F.,.F.,(4,1,1,
1,1,1,1,1,4),(279.601746169492,279.837227571946,280.836585705512,281.835943839078,
282.835301972644,283.83466010621,284.834018239776,285.833376373342,285.884931476671),
 .UNSPECIFIED.);
#438=B_SPLINE_CURVE_WITH_KNOTS('',3,(#19139,#19140,#19141,#19142,#19143,
#19144,#19145,#19146,#19147,#19148,#19149),.UNSPECIFIED.,.F.,.F.,(4,1,1,
1,1,1,1,1,4),(279.601746169492,279.807771486616,280.807129620182,281.806487753748,
282.805845887314,283.80520402088,284.804562154446,285.803920288012,285.884931476672),
 .UNSPECIFIED.);
#439=B_SPLINE_CURVE_WITH_KNOTS('',3,(#19154,#19155,#19156,#19157,#19158,
#19159,#19160,#19161,#19162,#19163),.UNSPECIFIED.,.F.,.F.,(4,1,1,1,1,1,
1,4),(273.318560862312,273.84107877055,274.840436904116,275.839795037682,
276.839153171248,277.838511304814,278.83786943838,279.601746169492),
 .UNSPECIFIED.);
#440=B_SPLINE_CURVE_WITH_KNOTS('',3,(#19164,#19165,#19166,#19167,#19168,
#19169,#19170,#19171,#19172,#19173),.UNSPECIFIED.,.F.,.F.,(4,1,1,1,1,1,
1,4),(273.318560862312,273.811622685219,274.810980818785,275.810338952351,
276.809697085917,277.809055219484,278.80841335305,279.601746169492),
 .UNSPECIFIED.);
#441=B_SPLINE_CURVE_WITH_KNOTS('',3,(#19178,#19179,#19180,#19181,#19182,
#19183,#19184,#19185,#19186,#19187),.UNSPECIFIED.,.F.,.F.,(4,1,1,1,1,1,
1,4),(267.035375555133,267.844929969153,268.844288102719,269.843646236285,
270.843004369851,271.842362503417,272.841720636983,273.318560862312),
 .UNSPECIFIED.);
#442=B_SPLINE_CURVE_WITH_KNOTS('',3,(#19188,#19189,#19190,#19191,#19192,
#19193,#19194,#19195,#19196,#19197),.UNSPECIFIED.,.F.,.F.,(4,1,1,1,1,1,
1,4),(267.035375555133,267.815473883823,268.814832017389,269.814190150955,
270.813548284521,271.812906418087,272.812264551653,273.318560862312),
 .UNSPECIFIED.);
#443=B_SPLINE_CURVE_WITH_KNOTS('',3,(#19202,#19203,#19204,#19205,#19206,
#19207,#19208,#19209,#19210,#19211,#19212),.UNSPECIFIED.,.F.,.F.,(4,1,1,
1,1,1,1,1,4),(260.752190247953,260.849423034191,261.848781167757,262.848139301323,
263.847497434889,264.846855568455,265.846213702021,266.845571835587,267.035375555133),
 .UNSPECIFIED.);
#444=B_SPLINE_CURVE_WITH_KNOTS('',3,(#19213,#19214,#19215,#19216,#19217,
#19218,#19219,#19220,#19221,#19222,#19223),.UNSPECIFIED.,.F.,.F.,(4,1,1,
1,1,1,1,1,4),(260.752190247953,260.819966948861,261.819325082427,262.818683215993,
263.818041349559,264.817399483125,265.816757616691,266.816115750257,267.035375555133),
 .UNSPECIFIED.);
#445=B_SPLINE_CURVE_WITH_KNOTS('',3,(#19228,#19229,#19230,#19231,#19232,
#19233,#19234,#19235,#19236,#19237),.UNSPECIFIED.,.F.,.F.,(4,1,1,1,1,1,
1,4),(254.469004940773,254.853274232795,255.852632366361,256.851990499927,
257.851348633493,258.850706767059,259.850064900625,260.752190247953),
 .UNSPECIFIED.);
#446=B_SPLINE_CURVE_WITH_KNOTS('',3,(#19238,#19239,#19240,#19241,#19242,
#19243,#19244,#19245,#19246,#19247),.UNSPECIFIED.,.F.,.F.,(4,1,1,1,1,1,
1,4),(254.469004940774,254.823818147464,255.82317628103,256.822534414597,
257.821892548163,258.821250681729,259.820608815295,260.752190247953),
 .UNSPECIFIED.);
#447=B_SPLINE_CURVE_WITH_KNOTS('',3,(#19252,#19253,#19254,#19255,#19256,
#19257,#19258,#19259,#19260,#19261),.UNSPECIFIED.,.F.,.F.,(4,1,1,1,1,1,
1,4),(248.185819633594,248.857125431398,249.856483564964,250.85584169853,
251.855199832097,252.854557965663,253.853916099229,254.469004940773),
 .UNSPECIFIED.);
#448=B_SPLINE_CURVE_WITH_KNOTS('',3,(#19262,#19263,#19264,#19265,#19266,
#19267,#19268,#19269,#19270,#19271),.UNSPECIFIED.,.F.,.F.,(4,1,1,1,1,1,
1,4),(248.185819633594,248.827669346068,249.827027479634,250.8263856132,
251.825743746766,252.825101880332,253.824460013898,254.469004940774),
 .UNSPECIFIED.);
#449=B_SPLINE_CURVE_WITH_KNOTS('',3,(#19276,#19277,#19278,#19279,#19280,
#19281,#19282,#19283,#19284,#19285),.UNSPECIFIED.,.F.,.F.,(4,1,1,1,1,1,
1,4),(241.902634326414,242.860976630002,243.860334763568,244.859692897134,
245.8590510307,246.858409164266,247.857767297832,248.185819633594),
 .UNSPECIFIED.);
#450=B_SPLINE_CURVE_WITH_KNOTS('',3,(#19286,#19287,#19288,#19289,#19290,
#19291,#19292,#19293,#19294,#19295),.UNSPECIFIED.,.F.,.F.,(4,1,1,1,1,1,
1,4),(241.902634326415,242.831520544672,243.830878678238,244.830236811804,
245.82959494537,246.828953078936,247.828311212502,248.185819633594),
 .UNSPECIFIED.);
#451=B_SPLINE_CURVE_WITH_KNOTS('',3,(#19300,#19301,#19302,#19303,#19304,
#19305,#19306,#19307,#19308,#19309,#19310),.UNSPECIFIED.,.F.,.F.,(4,1,1,
1,1,1,1,1,4),(235.619449019235,235.86546969504,236.864827828606,237.864185962172,
238.863544095738,239.862902229304,240.86226036287,241.861618496436,241.902634326414),
 .UNSPECIFIED.);
#452=B_SPLINE_CURVE_WITH_KNOTS('',3,(#19311,#19312,#19313,#19314,#19315,
#19316,#19317,#19318,#19319,#19320,#19321),.UNSPECIFIED.,.F.,.F.,(4,1,1,
1,1,1,1,1,4),(235.619449019235,235.83601360971,236.835371743276,237.834729876842,
238.834088010408,239.833446143974,240.83280427754,241.832162411106,241.902634326415),
 .UNSPECIFIED.);
#453=B_SPLINE_CURVE_WITH_KNOTS('',3,(#19326,#19327,#19328,#19329,#19330,
#19331,#19332,#19333,#19334,#19335),.UNSPECIFIED.,.F.,.F.,(4,1,1,1,1,1,
1,4),(229.336263712055,229.869320893643,230.86867902721,231.868037160776,
232.867395294342,233.866753427908,234.866111561474,235.619449019235),
 .UNSPECIFIED.);
#454=B_SPLINE_CURVE_WITH_KNOTS('',3,(#19336,#19337,#19338,#19339,#19340,
#19341,#19342,#19343,#19344,#19345),.UNSPECIFIED.,.F.,.F.,(4,1,1,1,1,1,
1,4),(229.336263712055,229.839864808313,230.839222941879,231.838581075445,
232.837939209011,233.837297342577,234.836655476144,235.619449019235),
 .UNSPECIFIED.);
#455=B_SPLINE_CURVE_WITH_KNOTS('',3,(#19350,#19351,#19352,#19353,#19354,
#19355,#19356,#19357,#19358,#19359),.UNSPECIFIED.,.F.,.F.,(4,1,1,1,1,1,
1,4),(223.053078404876,223.873172092247,224.872530225813,225.871888359379,
226.871246492945,227.870604626511,228.869962760077,229.336263712055),
 .UNSPECIFIED.);
#456=B_SPLINE_CURVE_WITH_KNOTS('',3,(#19360,#19361,#19362,#19363,#19364,
#19365,#19366,#19367,#19368,#19369),.UNSPECIFIED.,.F.,.F.,(4,1,1,1,1,1,
1,4),(223.053078404876,223.843716006917,224.843074140483,225.842432274049,
226.841790407615,227.841148541181,228.840506674747,229.336263712055),
 .UNSPECIFIED.);
#457=B_SPLINE_CURVE_WITH_KNOTS('',3,(#19374,#19375,#19376,#19377,#19378,
#19379,#19380,#19381,#19382,#19383,#19384),.UNSPECIFIED.,.F.,.F.,(4,1,1,
1,1,1,1,1,4),(216.769893097696,216.877665157285,217.877023290851,218.876381424417,
219.875739557983,220.875097691549,221.874455825115,222.873813958681,223.053078404876),
 .UNSPECIFIED.);
#458=B_SPLINE_CURVE_WITH_KNOTS('',3,(#19385,#19386,#19387,#19388,#19389,
#19390,#19391,#19392,#19393,#19394,#19395),.UNSPECIFIED.,.F.,.F.,(4,1,1,
1,1,1,1,1,4),(216.769893097696,216.848209071955,217.847567205521,218.846925339087,
219.846283472653,220.845641606219,221.844999739785,222.844357873351,223.053078404876),
 .UNSPECIFIED.);
#459=B_SPLINE_CURVE_WITH_KNOTS('',3,(#19400,#19401,#19402,#19403,#19404,
#19405,#19406,#19407,#19408,#19409),.UNSPECIFIED.,.F.,.F.,(4,1,1,1,1,1,
1,4),(210.486707790516,210.881516355889,211.880874489455,212.880232623021,
213.879590756587,214.878948890153,215.878307023719,216.769893097696),
 .UNSPECIFIED.);
#460=B_SPLINE_CURVE_WITH_KNOTS('',3,(#19410,#19411,#19412,#19413,#19414,
#19415,#19416,#19417,#19418,#19419),.UNSPECIFIED.,.F.,.F.,(4,1,1,1,1,1,
1,4),(210.486707790517,210.852060270558,211.851418404124,212.85077653769,
213.850134671257,214.849492804823,215.848850938389,216.769893097696),
 .UNSPECIFIED.);
#461=B_SPLINE_CURVE_WITH_KNOTS('',3,(#19424,#19425,#19426,#19427,#19428,
#19429,#19430,#19431,#19432,#19433),.UNSPECIFIED.,.F.,.F.,(4,1,1,1,1,1,
1,4),(204.203522483337,204.885367554492,205.884725688058,206.884083821624,
207.88344195519,208.882800088756,209.882158222323,210.486707790516),
 .UNSPECIFIED.);
#462=B_SPLINE_CURVE_WITH_KNOTS('',3,(#19434,#19435,#19436,#19437,#19438,
#19439,#19440,#19441,#19442,#19443),.UNSPECIFIED.,.F.,.F.,(4,1,1,1,1,1,
1,4),(204.203522483337,204.855911469162,205.855269602728,206.854627736294,
207.85398586986,208.853344003426,209.852702136992,210.486707790517),
 .UNSPECIFIED.);
#463=B_SPLINE_CURVE_WITH_KNOTS('',3,(#19448,#19449,#19450,#19451,#19452,
#19453,#19454,#19455,#19456,#19457),.UNSPECIFIED.,.F.,.F.,(4,1,1,1,1,1,
1,4),(197.920337176157,198.889218753096,199.888576886662,200.887935020228,
201.887293153794,202.88665128736,203.886009420926,204.203522483337),
 .UNSPECIFIED.);
#464=B_SPLINE_CURVE_WITH_KNOTS('',3,(#19458,#19459,#19460,#19461,#19462,
#19463,#19464,#19465,#19466,#19467),.UNSPECIFIED.,.F.,.F.,(4,1,1,1,1,1,
1,4),(197.920337176158,198.859762667766,199.859120801332,200.858478934898,
201.857837068464,202.85719520203,203.856553335596,204.203522483337),
 .UNSPECIFIED.);
#465=B_SPLINE_CURVE_WITH_KNOTS('',3,(#19472,#19473,#19474,#19475,#19476,
#19477,#19478,#19479,#19480,#19481,#19482),.UNSPECIFIED.,.F.,.F.,(4,1,1,
1,1,1,1,1,4),(191.637151868978,191.893711818134,192.8930699517,193.892428085266,
194.891786218832,195.891144352398,196.890502485964,197.88986061953,197.920337176157),
 .UNSPECIFIED.);
#466=B_SPLINE_CURVE_WITH_KNOTS('',3,(#19483,#19484,#19485,#19486,#19487,
#19488,#19489,#19490,#19491,#19492,#19493),.UNSPECIFIED.,.F.,.F.,(4,1,1,
1,1,1,1,1,4),(191.637151868978,191.864255732803,192.86361386637,193.862971999936,
194.862330133502,195.861688267068,196.861046400634,197.8604045342,197.920337176158),
 .UNSPECIFIED.);
#467=B_SPLINE_CURVE_WITH_KNOTS('',3,(#19498,#19499,#19500,#19501,#19502,
#19503,#19504,#19505,#19506,#19507),.UNSPECIFIED.,.F.,.F.,(4,1,1,1,1,1,
1,4),(185.353966561798,185.897563016737,186.896921150303,187.89627928387,
188.895637417436,189.894995551002,190.894353684568,191.637151868978),
 .UNSPECIFIED.);
#468=B_SPLINE_CURVE_WITH_KNOTS('',3,(#19508,#19509,#19510,#19511,#19512,
#19513,#19514,#19515,#19516,#19517),.UNSPECIFIED.,.F.,.F.,(4,1,1,1,1,1,
1,4),(185.353966561799,185.868106931407,186.867465064973,187.866823198539,
188.866181332105,189.865539465671,190.864897599237,191.637151868978),
 .UNSPECIFIED.);
#469=B_SPLINE_CURVE_WITH_KNOTS('',3,(#19522,#19523,#19524,#19525,#19526,
#19527,#19528,#19529,#19530,#19531),.UNSPECIFIED.,.F.,.F.,(4,1,1,1,1,1,
1,4),(179.070781254619,179.901414215341,180.900772348907,181.900130482473,
182.899488616039,183.898846749605,184.898204883171,185.353966561798),
 .UNSPECIFIED.);
#470=B_SPLINE_CURVE_WITH_KNOTS('',3,(#19532,#19533,#19534,#19535,#19536,
#19537,#19538,#19539,#19540,#19541),.UNSPECIFIED.,.F.,.F.,(4,1,1,1,1,1,
1,4),(179.070781254619,179.871958130011,180.871316263577,181.870674397143,
182.870032530709,183.869390664275,184.868748797841,185.353966561799),
 .UNSPECIFIED.);
#471=B_SPLINE_CURVE_WITH_KNOTS('',3,(#19546,#19547,#19548,#19549,#19550,
#19551,#19552,#19553,#19554,#19555,#19556),.UNSPECIFIED.,.F.,.F.,(4,1,1,
1,1,1,1,1,4),(172.787595947439,172.905907280379,173.905265413945,174.904623547511,
175.903981681077,176.903339814643,177.902697948209,178.902056081775,179.070781254619),
 .UNSPECIFIED.);
#472=B_SPLINE_CURVE_WITH_KNOTS('',3,(#19557,#19558,#19559,#19560,#19561,
#19562,#19563,#19564,#19565,#19566,#19567),.UNSPECIFIED.,.F.,.F.,(4,1,1,
1,1,1,1,1,4),(172.787595947439,172.876451195049,173.875809328615,174.875167462181,
175.874525595747,176.873883729313,177.873241862879,178.872599996445,179.070781254619),
 .UNSPECIFIED.);
#473=B_SPLINE_CURVE_WITH_KNOTS('',3,(#19572,#19573,#19574,#19575,#19576,
#19577,#19578,#19579,#19580,#19581),.UNSPECIFIED.,.F.,.F.,(4,1,1,1,1,1,
1,4),(166.504410640259,166.909758478983,167.909116612549,168.908474746115,
169.907832879681,170.907191013247,171.906549146813,172.787595947439),
 .UNSPECIFIED.);
#474=B_SPLINE_CURVE_WITH_KNOTS('',3,(#19582,#19583,#19584,#19585,#19586,
#19587,#19588,#19589,#19590,#19591),.UNSPECIFIED.,.F.,.F.,(4,1,1,1,1,1,
1,4),(166.50441064026,166.880302393652,167.879660527218,168.879018660784,
169.87837679435,170.877734927916,171.877093061483,172.787595947439),
 .UNSPECIFIED.);
#475=B_SPLINE_CURVE_WITH_KNOTS('',3,(#19596,#19597,#19598,#19599,#19600,
#19601,#19602,#19603,#19604,#19605),.UNSPECIFIED.,.F.,.F.,(4,1,1,1,1,1,
1,4),(160.22122533308,160.913609677586,161.912967811152,162.912325944718,
163.911684078284,164.91104221185,165.910400345416,166.504410640259),
 .UNSPECIFIED.);
#476=B_SPLINE_CURVE_WITH_KNOTS('',3,(#19606,#19607,#19608,#19609,#19610,
#19611,#19612,#19613,#19614,#19615),.UNSPECIFIED.,.F.,.F.,(4,1,1,1,1,1,
1,4),(160.22122533308,160.884153592256,161.883511725822,162.882869859388,
163.882227992954,164.88158612652,165.880944260086,166.50441064026),
 .UNSPECIFIED.);
#477=B_SPLINE_CURVE_WITH_KNOTS('',3,(#19620,#19621,#19622,#19623,#19624,
#19625,#19626,#19627,#19628,#19629),.UNSPECIFIED.,.F.,.F.,(4,1,1,1,1,1,
1,4),(153.9380400259,154.91746087619,155.916819009756,156.916177143322,
157.915535276888,158.914893410454,159.91425154402,160.22122533308),
 .UNSPECIFIED.);
#478=B_SPLINE_CURVE_WITH_KNOTS('',3,(#19630,#19631,#19632,#19633,#19634,
#19635,#19636,#19637,#19638,#19639),.UNSPECIFIED.,.F.,.F.,(4,1,1,1,1,1,
1,4),(153.938040025901,154.88800479086,155.887362924426,156.886721057992,
157.886079191558,158.885437325124,159.88479545869,160.22122533308),
 .UNSPECIFIED.);
#479=B_SPLINE_CURVE_WITH_KNOTS('',3,(#19644,#19645,#19646,#19647,#19648,
#19649,#19650,#19651,#19652,#19653,#19654),.UNSPECIFIED.,.F.,.F.,(4,1,1,
1,1,1,1,1,4),(147.654854718721,147.921953941228,148.921312074794,149.92067020836,
150.920028341926,151.919386475492,152.918744609058,153.918102742624,153.9380400259),
 .UNSPECIFIED.);
#480=B_SPLINE_CURVE_WITH_KNOTS('',3,(#19655,#19656,#19657,#19658,#19659,
#19660,#19661,#19662,#19663,#19664,#19665),.UNSPECIFIED.,.F.,.F.,(4,1,1,
1,1,1,1,1,4),(147.654854718721,147.892497855897,148.891855989463,149.891214123029,
150.890572256596,151.889930390162,152.889288523728,153.888646657294,153.938040025901),
 .UNSPECIFIED.);
#481=B_SPLINE_CURVE_WITH_KNOTS('',3,(#19670,#19671,#19672,#19673,#19674,
#19675,#19676,#19677,#19678,#19679),.UNSPECIFIED.,.F.,.F.,(4,1,1,1,1,1,
1,4),(141.371669411541,141.925805139831,142.925163273397,143.924521406963,
144.92387954053,145.923237674096,146.922595807662,147.654854718721),
 .UNSPECIFIED.);
#482=B_SPLINE_CURVE_WITH_KNOTS('',3,(#19680,#19681,#19682,#19683,#19684,
#19685,#19686,#19687,#19688,#19689),.UNSPECIFIED.,.F.,.F.,(4,1,1,1,1,1,
1,4),(141.371669411542,141.896349054501,142.895707188067,143.895065321633,
144.894423455199,145.893781588765,146.893139722331,147.654854718721),
 .UNSPECIFIED.);
#483=B_SPLINE_CURVE_WITH_KNOTS('',3,(#19694,#19695,#19696,#19697,#19698,
#19699,#19700,#19701,#19702,#19703),.UNSPECIFIED.,.F.,.F.,(4,1,1,1,1,1,
1,4),(135.088484104362,135.929656338435,136.929014472001,137.928372605567,
138.927730739133,139.927088872699,140.926447006265,141.371669411541),
 .UNSPECIFIED.);
#484=B_SPLINE_CURVE_WITH_KNOTS('',3,(#19704,#19705,#19706,#19707,#19708,
#19709,#19710,#19711,#19712,#19713),.UNSPECIFIED.,.F.,.F.,(4,1,1,1,1,1,
1,4),(135.088484104362,135.900200253105,136.899558386671,137.898916520237,
138.898274653803,139.897632787369,140.896990920935,141.371669411542),
 .UNSPECIFIED.);
#485=B_SPLINE_CURVE_WITH_KNOTS('',3,(#19718,#19719,#19720,#19721,#19722,
#19723,#19724,#19725,#19726,#19727,#19728),.UNSPECIFIED.,.F.,.F.,(4,1,1,
1,1,1,1,1,4),(128.805298797182,128.934149403473,129.933507537039,130.932865670605,
131.932223804171,132.931581937737,133.930940071303,134.930298204869,135.088484104362),
 .UNSPECIFIED.);
#486=B_SPLINE_CURVE_WITH_KNOTS('',3,(#19729,#19730,#19731,#19732,#19733,
#19734,#19735,#19736,#19737,#19738,#19739),.UNSPECIFIED.,.F.,.F.,(4,1,1,
1,1,1,1,1,4),(128.805298797182,128.904693318142,129.904051451709,130.903409585275,
131.902767718841,132.902125852407,133.901483985973,134.900842119539,135.088484104362),
 .UNSPECIFIED.);
#487=B_SPLINE_CURVE_WITH_KNOTS('',3,(#19744,#19745,#19746,#19747,#19748,
#19749,#19750,#19751,#19752,#19753),.UNSPECIFIED.,.F.,.F.,(4,1,1,1,1,1,
1,4),(122.522113490002,122.938000602077,123.937358735643,124.936716869209,
125.936075002775,126.935433136341,127.934791269907,128.805298797182),
 .UNSPECIFIED.);
#488=B_SPLINE_CURVE_WITH_KNOTS('',3,(#19754,#19755,#19756,#19757,#19758,
#19759,#19760,#19761,#19762,#19763),.UNSPECIFIED.,.F.,.F.,(4,1,1,1,1,1,
1,4),(122.522113490003,122.908544516746,123.907902650312,124.907260783878,
125.906618917444,126.90597705101,127.905335184576,128.805298797182),
 .UNSPECIFIED.);
#489=B_SPLINE_CURVE_WITH_KNOTS('',3,(#19768,#19769,#19770,#19771,#19772,
#19773,#19774,#19775,#19776,#19777),.UNSPECIFIED.,.F.,.F.,(4,1,1,1,1,1,
1,4),(116.238928182823,116.94185180068,117.941209934246,118.940568067812,
119.939926201378,120.939284334944,121.93864246851,122.522113490002),
 .UNSPECIFIED.);
#490=B_SPLINE_CURVE_WITH_KNOTS('',3,(#19778,#19779,#19780,#19781,#19782,
#19783,#19784,#19785,#19786,#19787),.UNSPECIFIED.,.F.,.F.,(4,1,1,1,1,1,
1,4),(116.238928182823,116.91239571535,117.911753848916,118.911111982482,
119.910470116048,120.909828249614,121.90918638318,122.522113490003),
 .UNSPECIFIED.);
#491=B_SPLINE_CURVE_WITH_KNOTS('',3,(#19792,#19793,#19794,#19795,#19796,
#19797,#19798,#19799,#19800,#19801),.UNSPECIFIED.,.F.,.F.,(4,1,1,1,1,1,
1,4),(109.955742875643,110.945702999284,111.94506113285,112.944419266416,
113.943777399982,114.943135533548,115.942493667114,116.238928182823),
 .UNSPECIFIED.);
#492=B_SPLINE_CURVE_WITH_KNOTS('',3,(#19802,#19803,#19804,#19805,#19806,
#19807,#19808,#19809,#19810,#19811),.UNSPECIFIED.,.F.,.F.,(4,1,1,1,1,1,
1,4),(109.955742875644,110.916246913954,111.91560504752,112.914963181086,
113.914321314652,114.913679448218,115.913037581784,116.238928182823),
 .UNSPECIFIED.);
#493=B_SPLINE_CURVE_WITH_KNOTS('',3,(#19816,#19817,#19818,#19819,#19820,
#19821,#19822,#19823,#19824,#19825,#19826),.UNSPECIFIED.,.F.,.F.,(4,1,1,
1,1,1,1,1,4),(103.672557568464,103.950196064322,104.949554197888,105.948912331454,
106.94827046502,107.947628598586,108.946986732152,109.946344865718,109.955742875643),
 .UNSPECIFIED.);
#494=B_SPLINE_CURVE_WITH_KNOTS('',3,(#19827,#19828,#19829,#19830,#19831,
#19832,#19833,#19834,#19835,#19836,#19837),.UNSPECIFIED.,.F.,.F.,(4,1,1,
1,1,1,1,1,4),(103.672557568464,103.920739978991,104.920098112557,105.919456246123,
106.918814379689,107.918172513255,108.917530646822,109.916888780388,109.955742875644),
 .UNSPECIFIED.);
#495=B_SPLINE_CURVE_WITH_KNOTS('',3,(#19842,#19843,#19844,#19845,#19846,
#19847,#19848,#19849,#19850,#19851),.UNSPECIFIED.,.F.,.F.,(4,1,1,1,1,1,
1,4),(97.3893722612841,97.9540472629253,98.9534053964914,99.9527635300574,
100.952121663623,101.95147979719,102.950837930756,103.672557568464),
 .UNSPECIFIED.);
#496=B_SPLINE_CURVE_WITH_KNOTS('',3,(#19852,#19853,#19854,#19855,#19856,
#19857,#19858,#19859,#19860,#19861),.UNSPECIFIED.,.F.,.F.,(4,1,1,1,1,1,
1,4),(97.3893722612845,97.924591177595,98.9239493111611,99.9233074447271,
100.922665578293,101.922023711859,102.921381845425,103.672557568464),
 .UNSPECIFIED.);
#497=B_SPLINE_CURVE_WITH_KNOTS('',3,(#19866,#19867,#19868,#19869,#19870,
#19871,#19872,#19873,#19874,#19875),.UNSPECIFIED.,.F.,.F.,(4,1,1,1,1,1,
1,4),(91.1061869541045,91.9578984615291,92.9572565950951,93.9566147286612,
94.9559728622272,95.9553309957932,96.9546891293593,97.3893722612841),
 .UNSPECIFIED.);
#498=B_SPLINE_CURVE_WITH_KNOTS('',3,(#19876,#19877,#19878,#19879,#19880,
#19881,#19882,#19883,#19884,#19885),.UNSPECIFIED.,.F.,.F.,(4,1,1,1,1,1,
1,4),(91.1061869541048,91.9284423761987,92.9278005097648,93.9271586433308,
94.9265167768969,95.9258749104629,96.925233044029,97.3893722612845),
 .UNSPECIFIED.);
#499=B_SPLINE_CURVE_WITH_KNOTS('',3,(#19890,#19891,#19892,#19893,#19894,
#19895,#19896,#19897,#19898,#19899,#19900),.UNSPECIFIED.,.F.,.F.,(4,1,1,
1,1,1,1,1,4),(84.8230016469249,84.9623915265667,85.9617496601328,86.9611077936988,
87.9604659272649,88.9598240608309,89.959182194397,90.958540327963,91.1061869541045),
 .UNSPECIFIED.);
#500=B_SPLINE_CURVE_WITH_KNOTS('',3,(#19901,#19902,#19903,#19904,#19905,
#19906,#19907,#19908,#19909,#19910,#19911),.UNSPECIFIED.,.F.,.F.,(4,1,1,
1,1,1,1,1,4),(84.8230016469253,84.9329354412364,85.9322935748025,86.9316517083685,
87.9310098419346,88.9303679755006,89.9297261090666,90.9290842426327,91.1061869541048),
 .UNSPECIFIED.);
#501=B_SPLINE_CURVE_WITH_KNOTS('',3,(#19916,#19917,#19918,#19919,#19920,
#19921,#19922,#19923,#19924,#19925),.UNSPECIFIED.,.F.,.F.,(4,1,1,1,1,1,
1,4),(78.5398163397454,78.9662427251705,79.9656008587365,80.9649589923026,
81.9643171258686,82.9636752594347,83.9630333930007,84.8230016469249),
 .UNSPECIFIED.);
#502=B_SPLINE_CURVE_WITH_KNOTS('',3,(#19926,#19927,#19928,#19929,#19930,
#19931,#19932,#19933,#19934,#19935),.UNSPECIFIED.,.F.,.F.,(4,1,1,1,1,1,
1,4),(78.5398163397457,78.9367866398401,79.9361447734062,80.9355029069722,
81.9348610405383,82.9342191741043,83.9335773076704,84.8230016469253),
 .UNSPECIFIED.);
#503=B_SPLINE_CURVE_WITH_KNOTS('',3,(#19940,#19941,#19942,#19943,#19944,
#19945,#19946,#19947,#19948,#19949),.UNSPECIFIED.,.F.,.F.,(4,1,1,1,1,1,
1,4),(72.2566310325658,72.9700939237742,73.9694520573402,74.9688101909063,
75.9681683244723,76.9675264580384,77.9668845916044,78.5398163397454),
 .UNSPECIFIED.);
#504=B_SPLINE_CURVE_WITH_KNOTS('',3,(#19950,#19951,#19952,#19953,#19954,
#19955,#19956,#19957,#19958,#19959),.UNSPECIFIED.,.F.,.F.,(4,1,1,1,1,1,
1,4),(72.2566310325661,72.9406378384438,73.9399959720099,74.9393541055759,
75.938712239142,76.938070372708,77.9374285062741,78.5398163397457),
 .UNSPECIFIED.);
#505=B_SPLINE_CURVE_WITH_KNOTS('',3,(#19964,#19965,#19966,#19967,#19968,
#19969,#19970,#19971,#19972,#19973,#19974),.UNSPECIFIED.,.F.,.F.,(4,1,1,
1,1,1,1,1,4),(65.9734457253862,65.9745869888119,66.9739451223779,67.9733032559439,
68.97266138951,69.972019523076,70.9713776566421,71.9707357902081,72.2566310325658),
 .UNSPECIFIED.);
#506=B_SPLINE_CURVE_WITH_KNOTS('',3,(#19975,#19976,#19977,#19978,#19979,
#19980,#19981,#19982,#19983,#19984),.UNSPECIFIED.,.F.,.F.,(4,1,1,1,1,1,
1,4),(65.9734457253865,66.9444890370476,67.9438471706136,68.9432053041797,
69.9425634377457,70.9419215713118,71.9412797048778,72.2566310325661),
 .UNSPECIFIED.);
#507=B_SPLINE_CURVE_WITH_KNOTS('',3,(#19989,#19990,#19991,#19992,#19993,
#19994,#19995,#19996,#19997,#19998,#19999,#20000),.UNSPECIFIED.,.F.,.F.,
(4,1,1,1,1,1,1,1,1,4),(59.6902604182066,59.9784381874156,60.4781172541986,
60.9777963209816,61.4774753877646,61.9771544545477,62.9765125881137,63.9758707216798,
64.9752288552458,65.9734457253862),.UNSPECIFIED.);
#508=B_SPLINE_CURVE_WITH_KNOTS('',3,(#20001,#20002,#20003,#20004,#20005,
#20006,#20007,#20008,#20009,#20010,#20011),.UNSPECIFIED.,.F.,.F.,(4,1,1,
1,1,1,1,1,4),(59.6902604182069,59.9489821020852,60.9483402356513,61.9476983692173,
62.9470565027834,63.9464146363494,64.9457727699155,65.9451309034815,65.9734457253865),
 .UNSPECIFIED.);
#509=B_SPLINE_CURVE_WITH_KNOTS('',3,(#20016,#20017,#20018,#20019,#20020,
#20021,#20022,#20023,#20024,#20025,#20026,#20027,#20028,#20029,#20030,#20031,
#20032),.UNSPECIFIED.,.F.,.F.,(4,1,1,1,1,1,1,1,1,1,1,1,1,1,4),(53.407075111027,
53.4826103192363,53.9822893860193,54.4819684528023,54.9816475195853,55.4813265863684,
55.9810056531514,56.4806847199344,56.9803637867174,57.4800428535005,57.9797219202835,
58.4794009870665,58.9790800538495,59.4787591206325,59.6902604182066),
 .UNSPECIFIED.);
#510=B_SPLINE_CURVE_WITH_KNOTS('',3,(#20033,#20034,#20035,#20036,#20037,
#20038,#20039,#20040,#20041,#20042,#20043,#20044,#20045,#20046,#20047,#20048),
 .UNSPECIFIED.,.F.,.F.,(4,1,1,1,1,1,1,1,1,1,1,1,1,4),(53.4070751110273,
53.4531542339059,53.9528333006889,54.452512367472,54.952191434255,55.451870501038,
55.951549567821,56.4512286346041,56.9509077013871,57.4505867681701,57.9502658349531,
58.4499449017362,58.9496239685192,59.6902604182069),.UNSPECIFIED.);
#511=B_SPLINE_CURVE_WITH_KNOTS('',3,(#20053,#20054,#20055,#20056,#20057,
#20058,#20059,#20060,#20061,#20062,#20063,#20064,#20065,#20066,#20067,#20068),
 .UNSPECIFIED.,.F.,.F.,(4,1,1,1,1,1,1,1,1,1,1,1,1,4),(47.1238898038474,
47.48646151784,47.986140584623,48.485819651406,48.9854987181891,49.4851777849721,
49.9848568517551,50.4845359185381,50.9842149853212,51.4838940521042,51.9835731188872,
52.4832521856702,52.9829312524532,53.407075111027),.UNSPECIFIED.);
#512=B_SPLINE_CURVE_WITH_KNOTS('',3,(#20069,#20070,#20071,#20072,#20073,
#20074,#20075,#20076,#20077,#20078,#20079,#20080,#20081,#20082,#20083,#20084),
 .UNSPECIFIED.,.F.,.F.,(4,1,1,1,1,1,1,1,1,1,1,1,1,4),(47.1238898038477,
47.4570054325096,47.9566844992927,48.4563635660757,48.9560426328587,49.4557216996417,
49.9554007664248,50.4550798332078,50.9547588999908,51.4544379667738,51.9541170335568,
52.4537961003399,52.9534751671229,53.4070751110273),.UNSPECIFIED.);
#513=B_SPLINE_CURVE_WITH_KNOTS('',3,(#20089,#20090,#20091,#20092,#20093,
#20094,#20095,#20096,#20097,#20098,#20099,#20100,#20101,#20102,#20103,#20104,
#20105),.UNSPECIFIED.,.F.,.F.,(4,1,1,1,1,1,1,1,1,1,1,1,1,1,4),(40.8407044966678,
40.9906336496607,41.4903127164437,41.9899917832267,42.4896708500098,42.9893499167928,
43.4890289835758,43.9887080503588,44.4883871171419,44.9880661839249,45.4877452507079,
45.9874243174909,46.4871033842739,46.986782451057,47.1238898038474),
 .UNSPECIFIED.);
#514=B_SPLINE_CURVE_WITH_KNOTS('',3,(#20106,#20107,#20108,#20109,#20110,
#20111,#20112,#20113,#20114,#20115,#20116,#20117,#20118,#20119,#20120,#20121,
#20122),.UNSPECIFIED.,.F.,.F.,(4,1,1,1,1,1,1,1,1,1,1,1,1,1,4),(40.8407044966681,
40.9611775643303,41.4608566311134,41.9605356978964,42.4602147646794,42.9598938314624,
43.4595728982454,43.9592519650285,44.4589310318115,44.9586100985945,45.4582891653775,
45.9579682321606,46.4576472989436,46.9573263657266,47.1238898038477),
 .UNSPECIFIED.);
#515=B_SPLINE_CURVE_WITH_KNOTS('',3,(#20127,#20128,#20129,#20130,#20131,
#20132,#20133,#20134,#20135,#20136,#20137,#20138,#20139,#20140,#20141,#20142),
 .UNSPECIFIED.,.F.,.F.,(4,1,1,1,1,1,1,1,1,1,1,1,1,4),(34.5575191894882,
34.9944848482644,35.4941639150474,35.9938429818305,36.4935220486135,36.9932011153965,
37.4928801821795,37.9925592489626,38.4922383157456,38.9919173825286,39.4915964493116,
39.9912755160946,40.4909545828777,40.8407044966678),.UNSPECIFIED.);
#516=B_SPLINE_CURVE_WITH_KNOTS('',3,(#20143,#20144,#20145,#20146,#20147,
#20148,#20149,#20150,#20151,#20152,#20153,#20154,#20155,#20156,#20157,#20158),
 .UNSPECIFIED.,.F.,.F.,(4,1,1,1,1,1,1,1,1,1,1,1,1,4),(34.5575191894886,
34.965028762934,35.4647078297171,35.9643868965001,36.4640659632831,36.9637450300661,
37.4634240968492,37.9631031636322,38.4627822304152,38.9624612971982,39.4621403639813,
39.9618194307643,40.4614984975473,40.8407044966681),.UNSPECIFIED.);
#517=B_SPLINE_CURVE_WITH_KNOTS('',3,(#20163,#20164,#20165,#20166,#20167,
#20168,#20169,#20170,#20171,#20172,#20173,#20174,#20175,#20176,#20177,#20178,
#20179),.UNSPECIFIED.,.F.,.F.,(4,1,1,1,1,1,1,1,1,1,1,1,1,1,4),(28.2743338823086,
28.4986569800851,28.9983360468681,29.4980151136512,29.9976941804342,30.4973732472172,
30.9970523140002,31.4967313807832,31.9964104475663,32.4960895143493,32.9957685811323,
33.4954476479153,33.9951267146984,34.4948057814814,34.5575191894882),
 .UNSPECIFIED.);
#518=B_SPLINE_CURVE_WITH_KNOTS('',3,(#20180,#20181,#20182,#20183,#20184,
#20185,#20186,#20187,#20188,#20189,#20190,#20191,#20192,#20193,#20194,#20195,
#20196),.UNSPECIFIED.,.F.,.F.,(4,1,1,1,1,1,1,1,1,1,1,1,1,1,4),(28.2743338823089,
28.4692008947547,28.9688799615378,29.4685590283208,29.9682380951038,30.4679171618868,
30.9675962286699,31.4672752954529,31.9669543622359,32.4666334290189,32.966312495802,
33.465991562585,33.965670629368,34.465349696151,34.5575191894886),
 .UNSPECIFIED.);
#519=B_SPLINE_CURVE_WITH_KNOTS('',3,(#20201,#20202,#20203,#20204,#20205,
#20206,#20207,#20208,#20209,#20210,#20211,#20212,#20213,#20214,#20215,#20216,
#20217),.UNSPECIFIED.,.F.,.F.,(4,1,1,1,1,1,1,1,1,1,1,1,1,1,4),(21.991148575129,
22.0028291119058,22.5025081786888,23.0021872454719,23.5018663122549,24.0015453790379,
24.5012244458209,25.0009035126039,25.500582579387,26.00026164617,26.499940712953,
26.999619779736,27.4992988465191,27.9989779133021,28.2743338823086),
 .UNSPECIFIED.);
#520=B_SPLINE_CURVE_WITH_KNOTS('',3,(#20218,#20219,#20220,#20221,#20222,
#20223,#20224,#20225,#20226,#20227,#20228,#20229,#20230,#20231,#20232,#20233),
 .UNSPECIFIED.,.F.,.F.,(4,1,1,1,1,1,1,1,1,1,1,1,1,4),(21.9911485751294,
22.4730520933585,22.9727311601415,23.4724102269245,23.9720892937075,24.4717683604905,
24.9714474272736,25.4711264940566,25.9708055608396,26.4704846276226,26.9701636944057,
27.4698427611887,27.9695218279717,28.2743338823089),.UNSPECIFIED.);
#521=B_SPLINE_CURVE_WITH_KNOTS('',3,(#20238,#20239,#20240,#20241,#20242,
#20243,#20244,#20245,#20246,#20247,#20248,#20249,#20250,#20251,#20252,#20253),
 .UNSPECIFIED.,.F.,.F.,(4,1,1,1,1,1,1,1,1,1,1,1,1,4),(15.7079632679495,
16.0066803105095,16.5063593772925,17.0060384440756,17.5057175108586,18.0053965776416,
18.5050756444246,19.0047547112077,19.5044337779907,20.0041128447737,20.5037919115567,
21.0034709783398,21.5031500451228,21.991148575129),.UNSPECIFIED.);
#522=B_SPLINE_CURVE_WITH_KNOTS('',3,(#20254,#20255,#20256,#20257,#20258,
#20259,#20260,#20261,#20262,#20263,#20264,#20265,#20266,#20267,#20268,#20269,
#20270),.UNSPECIFIED.,.F.,.F.,(4,1,1,1,1,1,1,1,1,1,1,1,1,1,4),(15.7079632679498,
15.9772242251791,16.4769032919622,16.9765823587452,17.4762614255282,17.9759404923112,
18.4756195590943,18.9752986258773,19.4749776926603,19.9746567594433,20.4743358262264,
20.9740148930094,21.4736939597924,21.9733730265754,21.9911485751294),
 .UNSPECIFIED.);
#523=B_SPLINE_CURVE_WITH_KNOTS('',3,(#22264,#22265,#22266,#22267,#22268,
#22269,#22270,#22271,#22272,#22273,#22274,#22275,#22276,#22277,#22278,#22279,
#22280,#22281,#22282,#22283,#22284,#22285,#22286,#22287,#22288,#22289,#22290,
#22291,#22292,#22293,#22294,#22295,#22296,#22297,#22298,#22299,#22300,#22301,
#22302,#22303),.UNSPECIFIED.,.F.,.F.,(4,3,3,3,3,3,3,3,3,3,3,3,3,4),(-0.53478501993692,
-0.534277081309421,-0.456439695901019,-0.38064245929011,-0.348102919117109,
-0.328886681298388,-0.258595553176405,-0.246742105655551,-0.185056579241663,
-0.163339235199672,-0.143463957830519,-0.0808484674142256,-0.0206857924044652,
0.),.UNSPECIFIED.);
#524=B_SPLINE_CURVE_WITH_KNOTS('',3,(#22304,#22305,#22306,#22307,#22308,
#22309,#22310,#22311,#22312,#22313,#22314,#22315,#22316,#22317,#22318,#22319,
#22320,#22321,#22322,#22323,#22324,#22325,#22326,#22327,#22328),
 .UNSPECIFIED.,.F.,.F.,(4,3,3,3,3,3,3,3,4),(390.000549715688,390.249351157541,
390.749030224325,391.248709291108,391.748388357891,392.248067424674,392.747746491457,
393.24742555824,393.746279249921),.UNSPECIFIED.);
#525=B_SPLINE_CURVE_WITH_KNOTS('',3,(#22330,#22331,#22332,#22333,#22334,
#22335,#22336,#22337,#22338,#22339,#22340,#22341,#22342,#22343,#22344,#22345,
#22346,#22347,#22348,#22349,#22350,#22351,#22352,#22353,#22354,#22355,#22356,
#22357,#22358,#22359,#22360,#22361,#22362,#22363,#22364,#22365,#22366),
 .UNSPECIFIED.,.F.,.F.,(4,3,3,3,3,3,3,3,3,3,3,3,4),(0.,0.000373494560508806,
0.0620760815771024,0.112839239637108,0.153038169722591,0.175804963675793,
0.247183842626883,0.319084136954533,0.344742425233931,0.363606980156396,
0.439518700737557,0.51795432283266,0.534785019937482),.UNSPECIFIED.);
#526=B_SPLINE_CURVE_WITH_KNOTS('',3,(#22367,#22368,#22369,#22370,#22371,
#22372,#22373,#22374,#22375,#22376,#22377,#22378,#22379,#22380,#22381),
 .UNSPECIFIED.,.F.,.F.,(4,1,1,1,1,1,1,1,1,1,1,1,4),(9.98190079888485,10.4807544905659,
10.9804335573489,11.4801126241319,11.979791690915,12.479470757698,12.979149824481,
13.478828891264,13.9785079580471,14.4781870248301,14.9778660916131,15.4775451583961,
15.7079632679498),.UNSPECIFIED.);
#527=B_SPLINE_CURVE_WITH_KNOTS('',3,(#22385,#22386,#22387,#22388,#22389,
#22390,#22391,#22392,#22393,#22394,#22395),.UNSPECIFIED.,.F.,.F.,(4,1,1,
1,1,1,1,1,4),(12.0092477762453,12.5089268430284,13.0086059098114,13.5082849765944,
14.0079640433774,14.5076431101605,15.0073221769435,15.5070012437265,15.7079632679495),
 .UNSPECIFIED.);
#528=B_SPLINE_CURVE_WITH_KNOTS('',3,(#24389,#24390,#24391,#24392,#24393,
#24394,#24395,#24396,#24397,#24398,#24399,#24400,#24401,#24402,#24403,#24404,
#24405,#24406,#24407,#24408,#24409,#24410,#24411,#24412,#24413,#24414,#24415,
#24416,#24417,#24418,#24419,#24420,#24421,#24422,#24423,#24424,#24425,#24426,
#24427,#24428),.UNSPECIFIED.,.F.,.F.,(4,3,3,3,3,3,3,3,3,3,3,3,3,4),(-0.539097184344981,
-0.538720824057998,-0.476544551511477,-0.429912347101587,-0.401091234701428,
-0.381803774975435,-0.313681369269712,-0.290015733871917,-0.24230273417063,
-0.214804629165427,-0.192593514291413,-0.116696500404398,-0.0381316372362206,
0.),.UNSPECIFIED.);
#529=B_SPLINE_CURVE_WITH_KNOTS('',3,(#24429,#24430,#24431,#24432,#24433,
#24434,#24435,#24436,#24437,#24438,#24439,#24440,#24441,#24442,#24443,#24444,
#24445,#24446,#24447,#24448,#24449,#24450,#24451,#24452,#24453,#24454,#24455,
#24456,#24457,#24458,#24459,#24460,#24461,#24462,#24463,#24464,#24465),
 .UNSPECIFIED.,.F.,.F.,(4,3,3,3,3,3,3,3,3,3,3,3,4),(0.,0.000511892384038064,
0.078754853834616,0.155070466132989,0.20164291816609,0.227017770490094,
0.290460834304131,0.352619921814331,0.383703668213755,0.403796492255862,
0.466621120797767,0.52704524650008,0.539097184344933),.UNSPECIFIED.);
#530=B_SPLINE_CURVE_WITH_KNOTS('',3,(#24466,#24467,#24468,#24469,#24470,
#24471,#24472,#24473,#24474,#24475),.UNSPECIFIED.,.F.,.F.,(4,3,3,4),(-394.746462758588,
-394.246783691805,-393.747104625022,-393.256204536838),.UNSPECIFIED.);
#531=B_SPLINE_CURVE_WITH_KNOTS('',3,(#24543,#24544,#24545,#24546,#24547,
#24548,#24549,#24550),.UNSPECIFIED.,.F.,.F.,(4,2,2,4),(0.756005737987019,
0.793568827564653,0.872922520054208,0.952276212543762),.UNSPECIFIED.);
#532=B_SPLINE_CURVE_WITH_KNOTS('',3,(#24553,#24554,#24555,#24556,#24557,
#24558,#24559,#24560,#24561,#24562,#24563,#24564,#24565,#24566),
 .UNSPECIFIED.,.F.,.F.,(4,2,2,2,2,2,4),(0.121154929624509,0.158718019202145,
0.238071711691699,0.317425404181254,0.396779096670809,0.476132789160363,
0.513695878738001),.UNSPECIFIED.);
#533=B_SPLINE_CURVE_WITH_KNOTS('',3,(#24567,#24568,#24569,#24570,#24571,
#24572,#24573,#24574),.UNSPECIFIED.,.F.,.F.,(4,2,2,4),(0.952276212543762,
1.03162990503332,1.11098359752287,1.14854668710052),.UNSPECIFIED.);
#534=B_SPLINE_CURVE_WITH_KNOTS('',3,(#24578,#24579,#24580,#24581,#24582,
#24583,#24584,#24585,#24586,#24587),.UNSPECIFIED.,.F.,.F.,(4,2,2,2,4),(0.,
0.0792165807733642,0.158433161546728,0.237648697074572,0.316864232602417),
 .UNSPECIFIED.);
#535=B_SPLINE_CURVE_WITH_KNOTS('',3,(#24588,#24589,#24590,#24591,#24592,
#24593,#24594,#24595,#24596,#24597,#24598,#24599,#24600,#24601,#24602,#24603,
#24604,#24605,#24606,#24607,#24608,#24609,#24610,#24611,#24612,#24613),
 .UNSPECIFIED.,.F.,.F.,(4,2,2,2,2,2,2,2,2,2,2,2,4),(0.316864232602417,0.396079768130261,
0.475295303658105,0.554511884431469,0.633728465204833,0.712945045978197,
0.792161626751562,0.871377162279406,0.95059269780725,1.02980823333509,1.10902376886294,
1.1882403496363,1.26745693040967),.UNSPECIFIED.);
#536=B_SPLINE_CURVE_WITH_KNOTS('',3,(#24645,#24646,#24647,#24648,#24649,
#24650),.UNSPECIFIED.,.F.,.F.,(4,2,4),(0.803821788694078,0.872950991853625,
0.952307212900975),.UNSPECIFIED.);
#537=B_SPLINE_CURVE_WITH_KNOTS('',3,(#24653,#24654,#24655,#24656,#24657,
#24658,#24659,#24660,#24661,#24662),.UNSPECIFIED.,.F.,.F.,(4,2,2,2,4),(0.168950313426762,
0.238079516586309,0.317435737633658,0.396791958681008,0.465921161840561),
 .UNSPECIFIED.);
#538=B_SPLINE_CURVE_WITH_KNOTS('',3,(#24663,#24664,#24665,#24666,#24667,
#24668),.UNSPECIFIED.,.F.,.F.,(4,2,4),(0.952307212900975,1.03166343394832,
1.10079263710787),.UNSPECIFIED.);
#539=B_SPLINE_CURVE_WITH_KNOTS('',3,(#24672,#24673,#24674,#24675,#24676,
#24677,#24678,#24679,#24680,#24681),.UNSPECIFIED.,.F.,.F.,(4,2,2,2,4),(0.,
0.0792165807733642,0.158433161546728,0.237648697074572,0.316864232602417),
 .UNSPECIFIED.);
#540=B_SPLINE_CURVE_WITH_KNOTS('',3,(#24682,#24683,#24684,#24685,#24686,
#24687,#24688,#24689,#24690,#24691,#24692,#24693,#24694,#24695,#24696,#24697,
#24698,#24699,#24700,#24701,#24702,#24703,#24704,#24705,#24706,#24707),
 .UNSPECIFIED.,.F.,.F.,(4,2,2,2,2,2,2,2,2,2,2,2,4),(0.316864232602417,0.396079768130261,
0.475295303658105,0.554511884431469,0.633728465204833,0.712945045978197,
0.792161626751562,0.871377162279406,0.95059269780725,1.02980823333509,1.10902376886294,
1.1882403496363,1.26745693040967),.UNSPECIFIED.);
#541=SPHERICAL_SURFACE('',#8614,0.3969);
#542=SPHERICAL_SURFACE('',#8616,0.3969);
#543=SPHERICAL_SURFACE('',#8618,0.3969);
#544=SPHERICAL_SURFACE('',#8620,0.3969);
#545=SPHERICAL_SURFACE('',#8622,0.3969);
#546=SPHERICAL_SURFACE('',#8624,0.3969);
#547=SPHERICAL_SURFACE('',#8626,0.3969);
#548=SPHERICAL_SURFACE('',#8628,0.3969);
#549=SPHERICAL_SURFACE('',#8631,0.412776);
#550=SPHERICAL_SURFACE('',#8647,0.412776);
#551=SPHERICAL_SURFACE('',#8652,0.412776);
#552=SPHERICAL_SURFACE('',#8657,0.412776);
#553=SPHERICAL_SURFACE('',#8662,0.412776);
#554=SPHERICAL_SURFACE('',#8667,0.412776);
#555=SPHERICAL_SURFACE('',#8672,0.412776);
#556=SPHERICAL_SURFACE('',#8680,0.412776);
#557=TOROIDAL_SURFACE('',#8574,1.675,0.412776);
#558=TOROIDAL_SURFACE('',#8594,1.675,0.412776);
#559=CONICAL_SURFACE('',#8561,0.475,0.785398163397449);
#560=CONICAL_SURFACE('',#8565,0.485,0.785398163397448);
#561=CONICAL_SURFACE('',#8569,0.31,0.463647609000806);
#562=CONICAL_SURFACE('',#8585,1.05,0.785398163397449);
#563=CONICAL_SURFACE('',#8592,1.05,0.785398163397449);
#564=CONICAL_SURFACE('',#8605,2.3,0.785398163397449);
#565=CONICAL_SURFACE('',#8609,2.3,0.785398163397449);
#566=CONICAL_SURFACE('',#8831,0.4,0.785398163397448);
#567=CONICAL_SURFACE('',#8835,0.41,0.785398163397448);
#568=CONICAL_SURFACE('',#8839,0.26,0.463647609000806);
#569=CONICAL_SURFACE('',#8843,0.225,0.785398163397448);
#570=CONICAL_SURFACE('',#8857,0.325,0.785398163397448);
#571=CONICAL_SURFACE('',#8861,0.335,0.785398163397448);
#572=CONICAL_SURFACE('',#8865,0.21,0.463647609000806);
#573=CONICAL_SURFACE('',#8869,0.18,0.785398163397448);
#574=CONICAL_SURFACE('',#9129,0.235,0.785398163397448);
#575=CONICAL_SURFACE('',#9133,0.2125,0.785398163397448);
#576=CONICAL_SURFACE('',#9148,0.475,0.785398163397449);
#577=CONICAL_SURFACE('',#9152,0.485,0.785398163397448);
#578=CONICAL_SURFACE('',#9156,0.31,0.463647609000806);
#579=CONICAL_SURFACE('',#9160,0.27,0.785398163397448);
#580=ORIENTED_CLOSED_SHELL('',*,#8058,.F.);
#581=ORIENTED_CLOSED_SHELL('',*,#8078,.F.);
#582=ORIENTED_CLOSED_SHELL('',*,#8080,.F.);
#583=ORIENTED_CLOSED_SHELL('',*,#8091,.F.);
#584=BREP_WITH_VOIDS('Body1',#8059,(#580));
#585=BREP_WITH_VOIDS('Body1',#8077,(#581));
#586=BREP_WITH_VOIDS('Body1',#8079,(#582));
#587=BREP_WITH_VOIDS('Body1',#8090,(#583));
#588=SHAPE_REPRESENTATION_RELATIONSHIP('SRR','None',#25196,#616);
#589=SHAPE_REPRESENTATION_RELATIONSHIP('SRR','None',#25197,#617);
#590=SHAPE_REPRESENTATION_RELATIONSHIP('SRR','None',#25198,#618);
#591=SHAPE_REPRESENTATION_RELATIONSHIP('SRR','None',#25199,#619);
#592=SHAPE_REPRESENTATION_RELATIONSHIP('SRR','None',#25200,#620);
#593=SHAPE_REPRESENTATION_RELATIONSHIP('SRR','None',#25201,#621);
#594=SHAPE_REPRESENTATION_RELATIONSHIP('SRR','None',#25202,#622);
#595=SHAPE_REPRESENTATION_RELATIONSHIP('SRR','None',#25204,#623);
#596=SHAPE_REPRESENTATION_RELATIONSHIP('SRR','None',#25205,#624);
#597=SHAPE_REPRESENTATION_RELATIONSHIP('SRR','None',#25206,#625);
#598=SHAPE_REPRESENTATION_RELATIONSHIP('SRR','None',#25207,#626);
#599=SHAPE_REPRESENTATION_RELATIONSHIP('SRR','None',#25208,#627);
#600=SHAPE_REPRESENTATION_RELATIONSHIP('SRR','None',#25210,#628);
#601=SHAPE_REPRESENTATION_RELATIONSHIP('SRR','None',#25211,#629);
#602=SHAPE_REPRESENTATION_RELATIONSHIP('SRR','None',#25212,#630);
#603=SHAPE_REPRESENTATION_RELATIONSHIP('SRR','None',#25213,#631);
#604=SHAPE_REPRESENTATION_RELATIONSHIP('SRR','None',#25214,#632);
#605=SHAPE_REPRESENTATION_RELATIONSHIP('SRR','None',#25215,#633);
#606=SHAPE_REPRESENTATION_RELATIONSHIP('SRR','None',#25217,#634);
#607=SHAPE_REPRESENTATION_RELATIONSHIP('SRR','None',#25218,#635);
#608=SHAPE_REPRESENTATION_RELATIONSHIP('SRR','None',#25219,#636);
#609=SHAPE_REPRESENTATION_RELATIONSHIP('SRR','None',#25220,#637);
#610=SHAPE_REPRESENTATION_RELATIONSHIP('SRR','None',#25221,#638);
#611=SHAPE_REPRESENTATION_RELATIONSHIP('SRR','None',#25222,#639);
#612=SHAPE_REPRESENTATION_RELATIONSHIP('SRR','None',#25223,#640);
#613=SHAPE_REPRESENTATION_RELATIONSHIP('SRR','None',#25224,#641);
#614=SHAPE_REPRESENTATION_RELATIONSHIP('SRR','None',#25225,#642);
#615=SHAPE_REPRESENTATION_RELATIONSHIP('SRR','None',#25226,#643);
#616=ADVANCED_BREP_SHAPE_REPRESENTATION('',(#680),#25043);
#617=ADVANCED_BREP_SHAPE_REPRESENTATION('',(#681),#25044);
#618=ADVANCED_BREP_SHAPE_REPRESENTATION('',(#682),#25045);
#619=ADVANCED_BREP_SHAPE_REPRESENTATION('',(#683),#25046);
#620=ADVANCED_BREP_SHAPE_REPRESENTATION('',(#684),#25047);
#621=ADVANCED_BREP_SHAPE_REPRESENTATION('',(#685),#25048);
#622=ADVANCED_BREP_SHAPE_REPRESENTATION('',(#584),#25049);
#623=ADVANCED_BREP_SHAPE_REPRESENTATION('',(#686),#25051);
#624=ADVANCED_BREP_SHAPE_REPRESENTATION('',(#687),#25052);
#625=ADVANCED_BREP_SHAPE_REPRESENTATION('',(#688,#689,#690,#691,#692,#693,
#694,#695),#25053);
#626=ADVANCED_BREP_SHAPE_REPRESENTATION('',(#696),#25054);
#627=ADVANCED_BREP_SHAPE_REPRESENTATION('',(#697,#698),#25055);
#628=ADVANCED_BREP_SHAPE_REPRESENTATION('',(#699),#25057);
#629=ADVANCED_BREP_SHAPE_REPRESENTATION('',(#700),#25058);
#630=ADVANCED_BREP_SHAPE_REPRESENTATION('',(#701),#25059);
#631=ADVANCED_BREP_SHAPE_REPRESENTATION('',(#702),#25060);
#632=ADVANCED_BREP_SHAPE_REPRESENTATION('',(#585),#25061);
#633=ADVANCED_BREP_SHAPE_REPRESENTATION('',(#586),#25062);
#634=ADVANCED_BREP_SHAPE_REPRESENTATION('',(#703),#25064);
#635=ADVANCED_BREP_SHAPE_REPRESENTATION('',(#704),#25065);
#636=ADVANCED_BREP_SHAPE_REPRESENTATION('',(#705),#25066);
#637=ADVANCED_BREP_SHAPE_REPRESENTATION('',(#706),#25067);
#638=ADVANCED_BREP_SHAPE_REPRESENTATION('',(#707),#25068);
#639=ADVANCED_BREP_SHAPE_REPRESENTATION('',(#708),#25069);
#640=ADVANCED_BREP_SHAPE_REPRESENTATION('',(#709),#25070);
#641=ADVANCED_BREP_SHAPE_REPRESENTATION('',(#710),#25071);
#642=ADVANCED_BREP_SHAPE_REPRESENTATION('',(#711),#25072);
#643=ADVANCED_BREP_SHAPE_REPRESENTATION('',(#587),#25073);
#644=STYLED_ITEM('',(#25418),#680);
#645=STYLED_ITEM('',(#25425),#681);
#646=STYLED_ITEM('',(#25425),#682);
#647=STYLED_ITEM('',(#25439),#683);
#648=STYLED_ITEM('',(#25439),#684);
#649=STYLED_ITEM('',(#25453),#685);
#650=STYLED_ITEM('',(#25446),#584);
#651=STYLED_ITEM('',(#25439),#686);
#652=STYLED_ITEM('',(#25439),#687);
#653=STYLED_ITEM('',(#25439),#688);
#654=STYLED_ITEM('',(#25439),#689);
#655=STYLED_ITEM('',(#25439),#690);
#656=STYLED_ITEM('',(#25439),#691);
#657=STYLED_ITEM('',(#25439),#692);
#658=STYLED_ITEM('',(#25439),#693);
#659=STYLED_ITEM('',(#25439),#694);
#660=STYLED_ITEM('',(#25439),#695);
#661=STYLED_ITEM('',(#25439),#696);
#662=STYLED_ITEM('',(#25439),#697);
#663=STYLED_ITEM('',(#25439),#698);
#664=STYLED_ITEM('',(#25432),#699);
#665=STYLED_ITEM('',(#25432),#700);
#666=STYLED_ITEM('',(#25453),#701);
#667=STYLED_ITEM('',(#25446),#702);
#668=STYLED_ITEM('',(#25446),#585);
#669=STYLED_ITEM('',(#25446),#586);
#670=STYLED_ITEM('',(#25446),#703);
#671=STYLED_ITEM('',(#25439),#704);
#672=STYLED_ITEM('',(#25439),#705);
#673=STYLED_ITEM('',(#25432),#706);
#674=STYLED_ITEM('',(#25432),#707);
#675=STYLED_ITEM('',(#25432),#708);
#676=STYLED_ITEM('',(#25439),#709);
#677=STYLED_ITEM('',(#25446),#710);
#678=STYLED_ITEM('',(#25446),#711);
#679=STYLED_ITEM('',(#25446),#587);
#680=MANIFOLD_SOLID_BREP('Body1',#8052);
#681=MANIFOLD_SOLID_BREP('Body1',#8053);
#682=MANIFOLD_SOLID_BREP('Body1',#8054);
#683=MANIFOLD_SOLID_BREP('Body1',#8055);
#684=MANIFOLD_SOLID_BREP('Body1',#8056);
#685=MANIFOLD_SOLID_BREP('Body1',#8057);
#686=MANIFOLD_SOLID_BREP('Body1',#8060);
#687=MANIFOLD_SOLID_BREP('Body1',#8061);
#688=MANIFOLD_SOLID_BREP('Body1',#8062);
#689=MANIFOLD_SOLID_BREP('Body2',#8063);
#690=MANIFOLD_SOLID_BREP('Body3',#8064);
#691=MANIFOLD_SOLID_BREP('Body4',#8065);
#692=MANIFOLD_SOLID_BREP('Body5',#8066);
#693=MANIFOLD_SOLID_BREP('Body6',#8067);
#694=MANIFOLD_SOLID_BREP('Body7',#8068);
#695=MANIFOLD_SOLID_BREP('Body8',#8069);
#696=MANIFOLD_SOLID_BREP('Continuous crown cage',#8070);
#697=MANIFOLD_SOLID_BREP('Body1',#8071);
#698=MANIFOLD_SOLID_BREP('Body2',#8072);
#699=MANIFOLD_SOLID_BREP('Body1',#8073);
#700=MANIFOLD_SOLID_BREP('Body1',#8074);
#701=MANIFOLD_SOLID_BREP('Body1',#8075);
#702=MANIFOLD_SOLID_BREP('Body1',#8076);
#703=MANIFOLD_SOLID_BREP('Body1',#8081);
#704=MANIFOLD_SOLID_BREP('Body1',#8082);
#705=MANIFOLD_SOLID_BREP('Body1',#8083);
#706=MANIFOLD_SOLID_BREP('Body1',#8084);
#707=MANIFOLD_SOLID_BREP('Body1',#8085);
#708=MANIFOLD_SOLID_BREP('Body1',#8086);
#709=MANIFOLD_SOLID_BREP('Body1',#8087);
#710=MANIFOLD_SOLID_BREP('Body1',#8088);
#711=MANIFOLD_SOLID_BREP('Body1',#8089);
#712=FACE_BOUND('',#1494,.T.);
#713=FACE_BOUND('',#1495,.T.);
#714=FACE_BOUND('',#1496,.T.);
#715=FACE_BOUND('',#1497,.T.);
#716=FACE_BOUND('',#1498,.T.);
#717=FACE_BOUND('',#1499,.T.);
#718=FACE_BOUND('',#1500,.T.);
#719=FACE_BOUND('',#1502,.T.);
#720=FACE_BOUND('',#1503,.T.);
#721=FACE_BOUND('',#1504,.T.);
#722=FACE_BOUND('',#1505,.T.);
#723=FACE_BOUND('',#1506,.T.);
#724=FACE_BOUND('',#1507,.T.);
#725=FACE_BOUND('',#1508,.T.);
#726=FACE_BOUND('',#1518,.T.);
#727=FACE_BOUND('',#1519,.T.);
#728=FACE_BOUND('',#1520,.T.);
#729=FACE_BOUND('',#1534,.T.);
#730=FACE_BOUND('',#1535,.T.);
#731=FACE_BOUND('',#1540,.T.);
#732=FACE_BOUND('',#1541,.T.);
#733=FACE_BOUND('',#1547,.T.);
#734=FACE_BOUND('',#1555,.T.);
#735=FACE_BOUND('',#1556,.T.);
#736=FACE_BOUND('',#1557,.T.);
#737=FACE_BOUND('',#1558,.T.);
#738=FACE_BOUND('',#1561,.T.);
#739=FACE_BOUND('',#1562,.T.);
#740=FACE_BOUND('',#1563,.T.);
#741=FACE_BOUND('',#1564,.T.);
#742=FACE_BOUND('',#1567,.T.);
#743=FACE_BOUND('',#1568,.T.);
#744=FACE_BOUND('',#1574,.T.);
#745=FACE_BOUND('',#1575,.T.);
#746=FACE_BOUND('',#1576,.T.);
#747=FACE_BOUND('',#1577,.T.);
#748=FACE_BOUND('',#1581,.T.);
#749=FACE_BOUND('',#1584,.T.);
#750=FACE_BOUND('',#1585,.T.);
#751=FACE_BOUND('',#1586,.T.);
#752=FACE_BOUND('',#1587,.T.);
#753=FACE_BOUND('',#1590,.T.);
#754=FACE_BOUND('',#1591,.T.);
#755=FACE_BOUND('',#1595,.T.);
#756=FACE_BOUND('',#1596,.T.);
#757=FACE_BOUND('',#1599,.T.);
#758=FACE_BOUND('',#1602,.T.);
#759=FACE_BOUND('',#1620,.T.);
#760=FACE_BOUND('',#1628,.T.);
#761=FACE_BOUND('',#1631,.T.);
#762=FACE_BOUND('',#1636,.T.);
#763=FACE_BOUND('',#1641,.T.);
#764=FACE_BOUND('',#1669,.T.);
#765=FACE_BOUND('',#1672,.T.);
#766=FACE_BOUND('',#1675,.T.);
#767=FACE_BOUND('',#1678,.T.);
#768=FACE_BOUND('',#1681,.T.);
#769=FACE_BOUND('',#1695,.T.);
#770=FACE_BOUND('',#1699,.T.);
#771=FACE_BOUND('',#1703,.T.);
#772=FACE_BOUND('',#1704,.T.);
#773=FACE_BOUND('',#1708,.T.);
#774=FACE_BOUND('',#1709,.T.);
#775=FACE_BOUND('',#1710,.T.);
#776=FACE_BOUND('',#1711,.T.);
#777=FACE_BOUND('',#1714,.T.);
#778=FACE_BOUND('',#1715,.T.);
#779=FACE_BOUND('',#1718,.T.);
#780=FACE_BOUND('',#1719,.T.);
#781=FACE_BOUND('',#1720,.T.);
#782=FACE_BOUND('',#1731,.T.);
#783=FACE_BOUND('',#1732,.T.);
#784=FACE_BOUND('',#1736,.T.);
#785=FACE_BOUND('',#1737,.T.);
#786=FACE_BOUND('',#1740,.T.);
#787=FACE_BOUND('',#1743,.T.);
#788=FACE_BOUND('',#1769,.T.);
#789=FACE_BOUND('',#1770,.T.);
#790=FACE_BOUND('',#1771,.T.);
#791=FACE_BOUND('',#1772,.T.);
#792=FACE_BOUND('',#1778,.T.);
#793=FACE_BOUND('',#1779,.T.);
#794=FACE_BOUND('',#1780,.T.);
#795=FACE_BOUND('',#1781,.T.);
#796=FACE_BOUND('',#1786,.T.);
#797=FACE_BOUND('',#1792,.T.);
#798=FACE_BOUND('',#1810,.T.);
#799=FACE_BOUND('',#1958,.T.);
#800=FACE_BOUND('',#1961,.T.);
#801=FACE_BOUND('',#1964,.T.);
#802=FACE_BOUND('',#1970,.T.);
#803=FACE_BOUND('',#1972,.T.);
#804=FACE_BOUND('',#1977,.T.);
#805=FACE_BOUND('',#1979,.T.);
#806=FACE_BOUND('',#1981,.T.);
#807=FACE_BOUND('',#1983,.T.);
#808=FACE_BOUND('',#1992,.T.);
#809=FACE_BOUND('',#1993,.T.);
#810=FACE_BOUND('',#1995,.T.);
#811=FACE_BOUND('',#1996,.T.);
#812=FACE_BOUND('',#1999,.T.);
#813=FACE_BOUND('',#2001,.T.);
#814=FACE_BOUND('',#2006,.T.);
#815=FACE_BOUND('',#2008,.T.);
#816=FACE_BOUND('',#2012,.T.);
#817=FACE_BOUND('',#2014,.T.);
#818=FACE_BOUND('',#2033,.T.);
#819=FACE_BOUND('',#2041,.T.);
#820=FACE_BOUND('',#2043,.T.);
#821=FACE_BOUND('',#2049,.T.);
#822=PLANE('',#8425);
#823=PLANE('',#8426);
#824=PLANE('',#8427);
#825=PLANE('',#8428);
#826=PLANE('',#8429);
#827=PLANE('',#8430);
#828=PLANE('',#8435);
#829=PLANE('',#8439);
#830=PLANE('',#8443);
#831=PLANE('',#8444);
#832=PLANE('',#8445);
#833=PLANE('',#8446);
#834=PLANE('',#8447);
#835=PLANE('',#8448);
#836=PLANE('',#8449);
#837=PLANE('',#8454);
#838=PLANE('',#8458);
#839=PLANE('',#8462);
#840=PLANE('',#8466);
#841=PLANE('',#8467);
#842=PLANE('',#8468);
#843=PLANE('',#8469);
#844=PLANE('',#8470);
#845=PLANE('',#8471);
#846=PLANE('',#8472);
#847=PLANE('',#8486);
#848=PLANE('',#8493);
#849=PLANE('',#8497);
#850=PLANE('',#8498);
#851=PLANE('',#8499);
#852=PLANE('',#8500);
#853=PLANE('',#8501);
#854=PLANE('',#8502);
#855=PLANE('',#8503);
#856=PLANE('',#8514);
#857=PLANE('',#8515);
#858=PLANE('',#8522);
#859=PLANE('',#8526);
#860=PLANE('',#8528);
#861=PLANE('',#8529);
#862=PLANE('',#8532);
#863=PLANE('',#8533);
#864=PLANE('',#8534);
#865=PLANE('',#8539);
#866=PLANE('',#8543);
#867=PLANE('',#8547);
#868=PLANE('',#8549);
#869=PLANE('',#8550);
#870=PLANE('',#8551);
#871=PLANE('',#8552);
#872=PLANE('',#8553);
#873=PLANE('',#8554);
#874=PLANE('',#8555);
#875=PLANE('',#8556);
#876=PLANE('',#8557);
#877=PLANE('',#8559);
#878=PLANE('',#8567);
#879=PLANE('',#8587);
#880=PLANE('',#8590);
#881=PLANE('',#8602);
#882=PLANE('',#8611);
#883=PLANE('',#8644);
#884=PLANE('',#8649);
#885=PLANE('',#8654);
#886=PLANE('',#8659);
#887=PLANE('',#8664);
#888=PLANE('',#8669);
#889=PLANE('',#8678);
#890=PLANE('',#8682);
#891=PLANE('',#8683);
#892=PLANE('',#8685);
#893=PLANE('',#8690);
#894=PLANE('',#8693);
#895=PLANE('',#8698);
#896=PLANE('',#8711);
#897=PLANE('',#8715);
#898=PLANE('',#8719);
#899=PLANE('',#8723);
#900=PLANE('',#8727);
#901=PLANE('',#8731);
#902=PLANE('',#8738);
#903=PLANE('',#8745);
#904=PLANE('',#8746);
#905=PLANE('',#8747);
#906=PLANE('',#8748);
#907=PLANE('',#8749);
#908=PLANE('',#8750);
#909=PLANE('',#8751);
#910=PLANE('',#8752);
#911=PLANE('',#8753);
#912=PLANE('',#8754);
#913=PLANE('',#8756);
#914=PLANE('',#8757);
#915=PLANE('',#8758);
#916=PLANE('',#8759);
#917=PLANE('',#8760);
#918=PLANE('',#8761);
#919=PLANE('',#8763);
#920=PLANE('',#8764);
#921=PLANE('',#8767);
#922=PLANE('',#8768);
#923=PLANE('',#8769);
#924=PLANE('',#8774);
#925=PLANE('',#8778);
#926=PLANE('',#8782);
#927=PLANE('',#8807);
#928=PLANE('',#8819);
#929=PLANE('',#8820);
#930=PLANE('',#8827);
#931=PLANE('',#8829);
#932=PLANE('',#8837);
#933=PLANE('',#8845);
#934=PLANE('',#8846);
#935=PLANE('',#8847);
#936=PLANE('',#8848);
#937=PLANE('',#8849);
#938=PLANE('',#8850);
#939=PLANE('',#8851);
#940=PLANE('',#8852);
#941=PLANE('',#8853);
#942=PLANE('',#8855);
#943=PLANE('',#8863);
#944=PLANE('',#8871);
#945=PLANE('',#8872);
#946=PLANE('',#8873);
#947=PLANE('',#8874);
#948=PLANE('',#8875);
#949=PLANE('',#8876);
#950=PLANE('',#8877);
#951=PLANE('',#8878);
#952=PLANE('',#8879);
#953=PLANE('',#9024);
#954=PLANE('',#9025);
#955=PLANE('',#9027);
#956=PLANE('',#9028);
#957=PLANE('',#9029);
#958=PLANE('',#9034);
#959=PLANE('',#9035);
#960=PLANE('',#9040);
#961=PLANE('',#9042);
#962=PLANE('',#9050);
#963=PLANE('',#9051);
#964=PLANE('',#9053);
#965=PLANE('',#9057);
#966=PLANE('',#9064);
#967=PLANE('',#9065);
#968=PLANE('',#9070);
#969=PLANE('',#9074);
#970=PLANE('',#9075);
#971=PLANE('',#9076);
#972=PLANE('',#9077);
#973=PLANE('',#9078);
#974=PLANE('',#9081);
#975=PLANE('',#9089);
#976=PLANE('',#9097);
#977=PLANE('',#9098);
#978=PLANE('',#9106);
#979=PLANE('',#9107);
#980=PLANE('',#9109);
#981=PLANE('',#9110);
#982=PLANE('',#9111);
#983=PLANE('',#9112);
#984=PLANE('',#9113);
#985=PLANE('',#9114);
#986=PLANE('',#9115);
#987=PLANE('',#9116);
#988=PLANE('',#9117);
#989=PLANE('',#9118);
#990=PLANE('',#9120);
#991=PLANE('',#9121);
#992=PLANE('',#9122);
#993=PLANE('',#9123);
#994=PLANE('',#9124);
#995=PLANE('',#9125);
#996=PLANE('',#9126);
#997=PLANE('',#9127);
#998=PLANE('',#9135);
#999=PLANE('',#9143);
#1000=PLANE('',#9144);
#1001=PLANE('',#9146);
#1002=PLANE('',#9154);
#1003=PLANE('',#9162);
#1004=PLANE('',#9163);
#1005=PLANE('',#9164);
#1006=PLANE('',#9165);
#1007=PLANE('',#9166);
#1008=PLANE('',#9167);
#1009=PLANE('',#9168);
#1010=PLANE('',#9169);
#1011=PLANE('',#9170);
#1012=FACE_OUTER_BOUND('',#1482,.T.);
#1013=FACE_OUTER_BOUND('',#1483,.T.);
#1014=FACE_OUTER_BOUND('',#1484,.T.);
#1015=FACE_OUTER_BOUND('',#1485,.T.);
#1016=FACE_OUTER_BOUND('',#1486,.T.);
#1017=FACE_OUTER_BOUND('',#1487,.T.);
#1018=FACE_OUTER_BOUND('',#1488,.T.);
#1019=FACE_OUTER_BOUND('',#1489,.T.);
#1020=FACE_OUTER_BOUND('',#1490,.T.);
#1021=FACE_OUTER_BOUND('',#1491,.T.);
#1022=FACE_OUTER_BOUND('',#1492,.T.);
#1023=FACE_OUTER_BOUND('',#1493,.T.);
#1024=FACE_OUTER_BOUND('',#1501,.T.);
#1025=FACE_OUTER_BOUND('',#1509,.T.);
#1026=FACE_OUTER_BOUND('',#1510,.T.);
#1027=FACE_OUTER_BOUND('',#1511,.T.);
#1028=FACE_OUTER_BOUND('',#1512,.T.);
#1029=FACE_OUTER_BOUND('',#1513,.T.);
#1030=FACE_OUTER_BOUND('',#1514,.T.);
#1031=FACE_OUTER_BOUND('',#1515,.T.);
#1032=FACE_OUTER_BOUND('',#1516,.T.);
#1033=FACE_OUTER_BOUND('',#1517,.T.);
#1034=FACE_OUTER_BOUND('',#1521,.T.);
#1035=FACE_OUTER_BOUND('',#1522,.T.);
#1036=FACE_OUTER_BOUND('',#1523,.T.);
#1037=FACE_OUTER_BOUND('',#1524,.T.);
#1038=FACE_OUTER_BOUND('',#1525,.T.);
#1039=FACE_OUTER_BOUND('',#1526,.T.);
#1040=FACE_OUTER_BOUND('',#1527,.T.);
#1041=FACE_OUTER_BOUND('',#1528,.T.);
#1042=FACE_OUTER_BOUND('',#1529,.T.);
#1043=FACE_OUTER_BOUND('',#1530,.T.);
#1044=FACE_OUTER_BOUND('',#1531,.T.);
#1045=FACE_OUTER_BOUND('',#1532,.T.);
#1046=FACE_OUTER_BOUND('',#1533,.T.);
#1047=FACE_OUTER_BOUND('',#1536,.T.);
#1048=FACE_OUTER_BOUND('',#1537,.T.);
#1049=FACE_OUTER_BOUND('',#1538,.T.);
#1050=FACE_OUTER_BOUND('',#1539,.T.);
#1051=FACE_OUTER_BOUND('',#1542,.T.);
#1052=FACE_OUTER_BOUND('',#1543,.T.);
#1053=FACE_OUTER_BOUND('',#1544,.T.);
#1054=FACE_OUTER_BOUND('',#1545,.T.);
#1055=FACE_OUTER_BOUND('',#1546,.T.);
#1056=FACE_OUTER_BOUND('',#1548,.T.);
#1057=FACE_OUTER_BOUND('',#1549,.T.);
#1058=FACE_OUTER_BOUND('',#1550,.T.);
#1059=FACE_OUTER_BOUND('',#1551,.T.);
#1060=FACE_OUTER_BOUND('',#1552,.T.);
#1061=FACE_OUTER_BOUND('',#1553,.T.);
#1062=FACE_OUTER_BOUND('',#1554,.T.);
#1063=FACE_OUTER_BOUND('',#1559,.T.);
#1064=FACE_OUTER_BOUND('',#1560,.T.);
#1065=FACE_OUTER_BOUND('',#1565,.T.);
#1066=FACE_OUTER_BOUND('',#1566,.T.);
#1067=FACE_OUTER_BOUND('',#1569,.T.);
#1068=FACE_OUTER_BOUND('',#1570,.T.);
#1069=FACE_OUTER_BOUND('',#1571,.T.);
#1070=FACE_OUTER_BOUND('',#1572,.T.);
#1071=FACE_OUTER_BOUND('',#1573,.T.);
#1072=FACE_OUTER_BOUND('',#1578,.T.);
#1073=FACE_OUTER_BOUND('',#1579,.T.);
#1074=FACE_OUTER_BOUND('',#1580,.T.);
#1075=FACE_OUTER_BOUND('',#1582,.T.);
#1076=FACE_OUTER_BOUND('',#1583,.T.);
#1077=FACE_OUTER_BOUND('',#1588,.T.);
#1078=FACE_OUTER_BOUND('',#1589,.T.);
#1079=FACE_OUTER_BOUND('',#1592,.T.);
#1080=FACE_OUTER_BOUND('',#1593,.T.);
#1081=FACE_OUTER_BOUND('',#1594,.T.);
#1082=FACE_OUTER_BOUND('',#1597,.T.);
#1083=FACE_OUTER_BOUND('',#1598,.T.);
#1084=FACE_OUTER_BOUND('',#1600,.T.);
#1085=FACE_OUTER_BOUND('',#1601,.T.);
#1086=FACE_OUTER_BOUND('',#1603,.T.);
#1087=FACE_OUTER_BOUND('',#1604,.T.);
#1088=FACE_OUTER_BOUND('',#1605,.T.);
#1089=FACE_OUTER_BOUND('',#1606,.T.);
#1090=FACE_OUTER_BOUND('',#1607,.T.);
#1091=FACE_OUTER_BOUND('',#1608,.T.);
#1092=FACE_OUTER_BOUND('',#1609,.T.);
#1093=FACE_OUTER_BOUND('',#1610,.T.);
#1094=FACE_OUTER_BOUND('',#1611,.T.);
#1095=FACE_OUTER_BOUND('',#1612,.T.);
#1096=FACE_OUTER_BOUND('',#1613,.T.);
#1097=FACE_OUTER_BOUND('',#1614,.T.);
#1098=FACE_OUTER_BOUND('',#1615,.T.);
#1099=FACE_OUTER_BOUND('',#1616,.T.);
#1100=FACE_OUTER_BOUND('',#1617,.T.);
#1101=FACE_OUTER_BOUND('',#1618,.T.);
#1102=FACE_OUTER_BOUND('',#1619,.T.);
#1103=FACE_OUTER_BOUND('',#1621,.T.);
#1104=FACE_OUTER_BOUND('',#1622,.T.);
#1105=FACE_OUTER_BOUND('',#1623,.T.);
#1106=FACE_OUTER_BOUND('',#1624,.T.);
#1107=FACE_OUTER_BOUND('',#1625,.T.);
#1108=FACE_OUTER_BOUND('',#1626,.T.);
#1109=FACE_OUTER_BOUND('',#1627,.T.);
#1110=FACE_OUTER_BOUND('',#1629,.T.);
#1111=FACE_OUTER_BOUND('',#1630,.T.);
#1112=FACE_OUTER_BOUND('',#1632,.T.);
#1113=FACE_OUTER_BOUND('',#1633,.T.);
#1114=FACE_OUTER_BOUND('',#1634,.T.);
#1115=FACE_OUTER_BOUND('',#1635,.T.);
#1116=FACE_OUTER_BOUND('',#1637,.T.);
#1117=FACE_OUTER_BOUND('',#1638,.T.);
#1118=FACE_OUTER_BOUND('',#1639,.T.);
#1119=FACE_OUTER_BOUND('',#1640,.T.);
#1120=FACE_OUTER_BOUND('',#1642,.T.);
#1121=FACE_OUTER_BOUND('',#1643,.T.);
#1122=FACE_OUTER_BOUND('',#1644,.T.);
#1123=FACE_OUTER_BOUND('',#1645,.T.);
#1124=FACE_OUTER_BOUND('',#1646,.T.);
#1125=FACE_OUTER_BOUND('',#1647,.T.);
#1126=FACE_OUTER_BOUND('',#1648,.T.);
#1127=FACE_OUTER_BOUND('',#1649,.T.);
#1128=FACE_OUTER_BOUND('',#1650,.T.);
#1129=FACE_OUTER_BOUND('',#1651,.T.);
#1130=FACE_OUTER_BOUND('',#1652,.T.);
#1131=FACE_OUTER_BOUND('',#1653,.T.);
#1132=FACE_OUTER_BOUND('',#1654,.T.);
#1133=FACE_OUTER_BOUND('',#1655,.T.);
#1134=FACE_OUTER_BOUND('',#1656,.T.);
#1135=FACE_OUTER_BOUND('',#1657,.T.);
#1136=FACE_OUTER_BOUND('',#1658,.T.);
#1137=FACE_OUTER_BOUND('',#1659,.T.);
#1138=FACE_OUTER_BOUND('',#1660,.T.);
#1139=FACE_OUTER_BOUND('',#1661,.T.);
#1140=FACE_OUTER_BOUND('',#1662,.T.);
#1141=FACE_OUTER_BOUND('',#1663,.T.);
#1142=FACE_OUTER_BOUND('',#1664,.T.);
#1143=FACE_OUTER_BOUND('',#1665,.T.);
#1144=FACE_OUTER_BOUND('',#1666,.T.);
#1145=FACE_OUTER_BOUND('',#1667,.T.);
#1146=FACE_OUTER_BOUND('',#1668,.T.);
#1147=FACE_OUTER_BOUND('',#1670,.T.);
#1148=FACE_OUTER_BOUND('',#1671,.T.);
#1149=FACE_OUTER_BOUND('',#1673,.T.);
#1150=FACE_OUTER_BOUND('',#1674,.T.);
#1151=FACE_OUTER_BOUND('',#1676,.T.);
#1152=FACE_OUTER_BOUND('',#1677,.T.);
#1153=FACE_OUTER_BOUND('',#1679,.T.);
#1154=FACE_OUTER_BOUND('',#1680,.T.);
#1155=FACE_OUTER_BOUND('',#1682,.T.);
#1156=FACE_OUTER_BOUND('',#1683,.T.);
#1157=FACE_OUTER_BOUND('',#1684,.T.);
#1158=FACE_OUTER_BOUND('',#1685,.T.);
#1159=FACE_OUTER_BOUND('',#1686,.T.);
#1160=FACE_OUTER_BOUND('',#1687,.T.);
#1161=FACE_OUTER_BOUND('',#1688,.T.);
#1162=FACE_OUTER_BOUND('',#1689,.T.);
#1163=FACE_OUTER_BOUND('',#1690,.T.);
#1164=FACE_OUTER_BOUND('',#1691,.T.);
#1165=FACE_OUTER_BOUND('',#1692,.T.);
#1166=FACE_OUTER_BOUND('',#1693,.T.);
#1167=FACE_OUTER_BOUND('',#1694,.T.);
#1168=FACE_OUTER_BOUND('',#1696,.T.);
#1169=FACE_OUTER_BOUND('',#1697,.T.);
#1170=FACE_OUTER_BOUND('',#1698,.T.);
#1171=FACE_OUTER_BOUND('',#1700,.T.);
#1172=FACE_OUTER_BOUND('',#1701,.T.);
#1173=FACE_OUTER_BOUND('',#1702,.T.);
#1174=FACE_OUTER_BOUND('',#1705,.T.);
#1175=FACE_OUTER_BOUND('',#1706,.T.);
#1176=FACE_OUTER_BOUND('',#1707,.T.);
#1177=FACE_OUTER_BOUND('',#1712,.T.);
#1178=FACE_OUTER_BOUND('',#1713,.T.);
#1179=FACE_OUTER_BOUND('',#1716,.T.);
#1180=FACE_OUTER_BOUND('',#1717,.T.);
#1181=FACE_OUTER_BOUND('',#1721,.T.);
#1182=FACE_OUTER_BOUND('',#1722,.T.);
#1183=FACE_OUTER_BOUND('',#1723,.T.);
#1184=FACE_OUTER_BOUND('',#1724,.T.);
#1185=FACE_OUTER_BOUND('',#1725,.T.);
#1186=FACE_OUTER_BOUND('',#1726,.T.);
#1187=FACE_OUTER_BOUND('',#1727,.T.);
#1188=FACE_OUTER_BOUND('',#1728,.T.);
#1189=FACE_OUTER_BOUND('',#1729,.T.);
#1190=FACE_OUTER_BOUND('',#1730,.T.);
#1191=FACE_OUTER_BOUND('',#1733,.T.);
#1192=FACE_OUTER_BOUND('',#1734,.T.);
#1193=FACE_OUTER_BOUND('',#1735,.T.);
#1194=FACE_OUTER_BOUND('',#1738,.T.);
#1195=FACE_OUTER_BOUND('',#1739,.T.);
#1196=FACE_OUTER_BOUND('',#1741,.T.);
#1197=FACE_OUTER_BOUND('',#1742,.T.);
#1198=FACE_OUTER_BOUND('',#1744,.T.);
#1199=FACE_OUTER_BOUND('',#1745,.T.);
#1200=FACE_OUTER_BOUND('',#1746,.T.);
#1201=FACE_OUTER_BOUND('',#1747,.T.);
#1202=FACE_OUTER_BOUND('',#1748,.T.);
#1203=FACE_OUTER_BOUND('',#1749,.T.);
#1204=FACE_OUTER_BOUND('',#1750,.T.);
#1205=FACE_OUTER_BOUND('',#1751,.T.);
#1206=FACE_OUTER_BOUND('',#1752,.T.);
#1207=FACE_OUTER_BOUND('',#1753,.T.);
#1208=FACE_OUTER_BOUND('',#1754,.T.);
#1209=FACE_OUTER_BOUND('',#1755,.T.);
#1210=FACE_OUTER_BOUND('',#1756,.T.);
#1211=FACE_OUTER_BOUND('',#1757,.T.);
#1212=FACE_OUTER_BOUND('',#1758,.T.);
#1213=FACE_OUTER_BOUND('',#1759,.T.);
#1214=FACE_OUTER_BOUND('',#1760,.T.);
#1215=FACE_OUTER_BOUND('',#1761,.T.);
#1216=FACE_OUTER_BOUND('',#1762,.T.);
#1217=FACE_OUTER_BOUND('',#1763,.T.);
#1218=FACE_OUTER_BOUND('',#1764,.T.);
#1219=FACE_OUTER_BOUND('',#1765,.T.);
#1220=FACE_OUTER_BOUND('',#1766,.T.);
#1221=FACE_OUTER_BOUND('',#1767,.T.);
#1222=FACE_OUTER_BOUND('',#1768,.T.);
#1223=FACE_OUTER_BOUND('',#1773,.T.);
#1224=FACE_OUTER_BOUND('',#1774,.T.);
#1225=FACE_OUTER_BOUND('',#1775,.T.);
#1226=FACE_OUTER_BOUND('',#1776,.T.);
#1227=FACE_OUTER_BOUND('',#1777,.T.);
#1228=FACE_OUTER_BOUND('',#1782,.T.);
#1229=FACE_OUTER_BOUND('',#1783,.T.);
#1230=FACE_OUTER_BOUND('',#1784,.T.);
#1231=FACE_OUTER_BOUND('',#1785,.T.);
#1232=FACE_OUTER_BOUND('',#1787,.T.);
#1233=FACE_OUTER_BOUND('',#1788,.T.);
#1234=FACE_OUTER_BOUND('',#1789,.T.);
#1235=FACE_OUTER_BOUND('',#1790,.T.);
#1236=FACE_OUTER_BOUND('',#1791,.T.);
#1237=FACE_OUTER_BOUND('',#1793,.T.);
#1238=FACE_OUTER_BOUND('',#1794,.T.);
#1239=FACE_OUTER_BOUND('',#1795,.T.);
#1240=FACE_OUTER_BOUND('',#1796,.T.);
#1241=FACE_OUTER_BOUND('',#1797,.T.);
#1242=FACE_OUTER_BOUND('',#1798,.T.);
#1243=FACE_OUTER_BOUND('',#1799,.T.);
#1244=FACE_OUTER_BOUND('',#1800,.T.);
#1245=FACE_OUTER_BOUND('',#1801,.T.);
#1246=FACE_OUTER_BOUND('',#1802,.T.);
#1247=FACE_OUTER_BOUND('',#1803,.T.);
#1248=FACE_OUTER_BOUND('',#1804,.T.);
#1249=FACE_OUTER_BOUND('',#1805,.T.);
#1250=FACE_OUTER_BOUND('',#1806,.T.);
#1251=FACE_OUTER_BOUND('',#1807,.T.);
#1252=FACE_OUTER_BOUND('',#1808,.T.);
#1253=FACE_OUTER_BOUND('',#1809,.T.);
#1254=FACE_OUTER_BOUND('',#1811,.T.);
#1255=FACE_OUTER_BOUND('',#1812,.T.);
#1256=FACE_OUTER_BOUND('',#1813,.T.);
#1257=FACE_OUTER_BOUND('',#1814,.T.);
#1258=FACE_OUTER_BOUND('',#1815,.T.);
#1259=FACE_OUTER_BOUND('',#1816,.T.);
#1260=FACE_OUTER_BOUND('',#1817,.T.);
#1261=FACE_OUTER_BOUND('',#1818,.T.);
#1262=FACE_OUTER_BOUND('',#1819,.T.);
#1263=FACE_OUTER_BOUND('',#1820,.T.);
#1264=FACE_OUTER_BOUND('',#1821,.T.);
#1265=FACE_OUTER_BOUND('',#1822,.T.);
#1266=FACE_OUTER_BOUND('',#1823,.T.);
#1267=FACE_OUTER_BOUND('',#1824,.T.);
#1268=FACE_OUTER_BOUND('',#1825,.T.);
#1269=FACE_OUTER_BOUND('',#1826,.T.);
#1270=FACE_OUTER_BOUND('',#1827,.T.);
#1271=FACE_OUTER_BOUND('',#1828,.T.);
#1272=FACE_OUTER_BOUND('',#1829,.T.);
#1273=FACE_OUTER_BOUND('',#1830,.T.);
#1274=FACE_OUTER_BOUND('',#1831,.T.);
#1275=FACE_OUTER_BOUND('',#1832,.T.);
#1276=FACE_OUTER_BOUND('',#1833,.T.);
#1277=FACE_OUTER_BOUND('',#1834,.T.);
#1278=FACE_OUTER_BOUND('',#1835,.T.);
#1279=FACE_OUTER_BOUND('',#1836,.T.);
#1280=FACE_OUTER_BOUND('',#1837,.T.);
#1281=FACE_OUTER_BOUND('',#1838,.T.);
#1282=FACE_OUTER_BOUND('',#1839,.T.);
#1283=FACE_OUTER_BOUND('',#1840,.T.);
#1284=FACE_OUTER_BOUND('',#1841,.T.);
#1285=FACE_OUTER_BOUND('',#1842,.T.);
#1286=FACE_OUTER_BOUND('',#1843,.T.);
#1287=FACE_OUTER_BOUND('',#1844,.T.);
#1288=FACE_OUTER_BOUND('',#1845,.T.);
#1289=FACE_OUTER_BOUND('',#1846,.T.);
#1290=FACE_OUTER_BOUND('',#1847,.T.);
#1291=FACE_OUTER_BOUND('',#1848,.T.);
#1292=FACE_OUTER_BOUND('',#1849,.T.);
#1293=FACE_OUTER_BOUND('',#1850,.T.);
#1294=FACE_OUTER_BOUND('',#1851,.T.);
#1295=FACE_OUTER_BOUND('',#1852,.T.);
#1296=FACE_OUTER_BOUND('',#1853,.T.);
#1297=FACE_OUTER_BOUND('',#1854,.T.);
#1298=FACE_OUTER_BOUND('',#1855,.T.);
#1299=FACE_OUTER_BOUND('',#1856,.T.);
#1300=FACE_OUTER_BOUND('',#1857,.T.);
#1301=FACE_OUTER_BOUND('',#1858,.T.);
#1302=FACE_OUTER_BOUND('',#1859,.T.);
#1303=FACE_OUTER_BOUND('',#1860,.T.);
#1304=FACE_OUTER_BOUND('',#1861,.T.);
#1305=FACE_OUTER_BOUND('',#1862,.T.);
#1306=FACE_OUTER_BOUND('',#1863,.T.);
#1307=FACE_OUTER_BOUND('',#1864,.T.);
#1308=FACE_OUTER_BOUND('',#1865,.T.);
#1309=FACE_OUTER_BOUND('',#1866,.T.);
#1310=FACE_OUTER_BOUND('',#1867,.T.);
#1311=FACE_OUTER_BOUND('',#1868,.T.);
#1312=FACE_OUTER_BOUND('',#1869,.T.);
#1313=FACE_OUTER_BOUND('',#1870,.T.);
#1314=FACE_OUTER_BOUND('',#1871,.T.);
#1315=FACE_OUTER_BOUND('',#1872,.T.);
#1316=FACE_OUTER_BOUND('',#1873,.T.);
#1317=FACE_OUTER_BOUND('',#1874,.T.);
#1318=FACE_OUTER_BOUND('',#1875,.T.);
#1319=FACE_OUTER_BOUND('',#1876,.T.);
#1320=FACE_OUTER_BOUND('',#1877,.T.);
#1321=FACE_OUTER_BOUND('',#1878,.T.);
#1322=FACE_OUTER_BOUND('',#1879,.T.);
#1323=FACE_OUTER_BOUND('',#1880,.T.);
#1324=FACE_OUTER_BOUND('',#1881,.T.);
#1325=FACE_OUTER_BOUND('',#1882,.T.);
#1326=FACE_OUTER_BOUND('',#1883,.T.);
#1327=FACE_OUTER_BOUND('',#1884,.T.);
#1328=FACE_OUTER_BOUND('',#1885,.T.);
#1329=FACE_OUTER_BOUND('',#1886,.T.);
#1330=FACE_OUTER_BOUND('',#1887,.T.);
#1331=FACE_OUTER_BOUND('',#1888,.T.);
#1332=FACE_OUTER_BOUND('',#1889,.T.);
#1333=FACE_OUTER_BOUND('',#1890,.T.);
#1334=FACE_OUTER_BOUND('',#1891,.T.);
#1335=FACE_OUTER_BOUND('',#1892,.T.);
#1336=FACE_OUTER_BOUND('',#1893,.T.);
#1337=FACE_OUTER_BOUND('',#1894,.T.);
#1338=FACE_OUTER_BOUND('',#1895,.T.);
#1339=FACE_OUTER_BOUND('',#1896,.T.);
#1340=FACE_OUTER_BOUND('',#1897,.T.);
#1341=FACE_OUTER_BOUND('',#1898,.T.);
#1342=FACE_OUTER_BOUND('',#1899,.T.);
#1343=FACE_OUTER_BOUND('',#1900,.T.);
#1344=FACE_OUTER_BOUND('',#1901,.T.);
#1345=FACE_OUTER_BOUND('',#1902,.T.);
#1346=FACE_OUTER_BOUND('',#1903,.T.);
#1347=FACE_OUTER_BOUND('',#1904,.T.);
#1348=FACE_OUTER_BOUND('',#1905,.T.);
#1349=FACE_OUTER_BOUND('',#1906,.T.);
#1350=FACE_OUTER_BOUND('',#1907,.T.);
#1351=FACE_OUTER_BOUND('',#1908,.T.);
#1352=FACE_OUTER_BOUND('',#1909,.T.);
#1353=FACE_OUTER_BOUND('',#1910,.T.);
#1354=FACE_OUTER_BOUND('',#1911,.T.);
#1355=FACE_OUTER_BOUND('',#1912,.T.);
#1356=FACE_OUTER_BOUND('',#1913,.T.);
#1357=FACE_OUTER_BOUND('',#1914,.T.);
#1358=FACE_OUTER_BOUND('',#1915,.T.);
#1359=FACE_OUTER_BOUND('',#1916,.T.);
#1360=FACE_OUTER_BOUND('',#1917,.T.);
#1361=FACE_OUTER_BOUND('',#1918,.T.);
#1362=FACE_OUTER_BOUND('',#1919,.T.);
#1363=FACE_OUTER_BOUND('',#1920,.T.);
#1364=FACE_OUTER_BOUND('',#1921,.T.);
#1365=FACE_OUTER_BOUND('',#1922,.T.);
#1366=FACE_OUTER_BOUND('',#1923,.T.);
#1367=FACE_OUTER_BOUND('',#1924,.T.);
#1368=FACE_OUTER_BOUND('',#1925,.T.);
#1369=FACE_OUTER_BOUND('',#1926,.T.);
#1370=FACE_OUTER_BOUND('',#1927,.T.);
#1371=FACE_OUTER_BOUND('',#1928,.T.);
#1372=FACE_OUTER_BOUND('',#1929,.T.);
#1373=FACE_OUTER_BOUND('',#1930,.T.);
#1374=FACE_OUTER_BOUND('',#1931,.T.);
#1375=FACE_OUTER_BOUND('',#1932,.T.);
#1376=FACE_OUTER_BOUND('',#1933,.T.);
#1377=FACE_OUTER_BOUND('',#1934,.T.);
#1378=FACE_OUTER_BOUND('',#1935,.T.);
#1379=FACE_OUTER_BOUND('',#1936,.T.);
#1380=FACE_OUTER_BOUND('',#1937,.T.);
#1381=FACE_OUTER_BOUND('',#1938,.T.);
#1382=FACE_OUTER_BOUND('',#1939,.T.);
#1383=FACE_OUTER_BOUND('',#1940,.T.);
#1384=FACE_OUTER_BOUND('',#1941,.T.);
#1385=FACE_OUTER_BOUND('',#1942,.T.);
#1386=FACE_OUTER_BOUND('',#1943,.T.);
#1387=FACE_OUTER_BOUND('',#1944,.T.);
#1388=FACE_OUTER_BOUND('',#1945,.T.);
#1389=FACE_OUTER_BOUND('',#1946,.T.);
#1390=FACE_OUTER_BOUND('',#1947,.T.);
#1391=FACE_OUTER_BOUND('',#1948,.T.);
#1392=FACE_OUTER_BOUND('',#1949,.T.);
#1393=FACE_OUTER_BOUND('',#1950,.T.);
#1394=FACE_OUTER_BOUND('',#1951,.T.);
#1395=FACE_OUTER_BOUND('',#1952,.T.);
#1396=FACE_OUTER_BOUND('',#1953,.T.);
#1397=FACE_OUTER_BOUND('',#1954,.T.);
#1398=FACE_OUTER_BOUND('',#1955,.T.);
#1399=FACE_OUTER_BOUND('',#1956,.T.);
#1400=FACE_OUTER_BOUND('',#1957,.T.);
#1401=FACE_OUTER_BOUND('',#1959,.T.);
#1402=FACE_OUTER_BOUND('',#1960,.T.);
#1403=FACE_OUTER_BOUND('',#1962,.T.);
#1404=FACE_OUTER_BOUND('',#1963,.T.);
#1405=FACE_OUTER_BOUND('',#1965,.T.);
#1406=FACE_OUTER_BOUND('',#1966,.T.);
#1407=FACE_OUTER_BOUND('',#1967,.T.);
#1408=FACE_OUTER_BOUND('',#1968,.T.);
#1409=FACE_OUTER_BOUND('',#1969,.T.);
#1410=FACE_OUTER_BOUND('',#1971,.T.);
#1411=FACE_OUTER_BOUND('',#1973,.T.);
#1412=FACE_OUTER_BOUND('',#1974,.T.);
#1413=FACE_OUTER_BOUND('',#1975,.T.);
#1414=FACE_OUTER_BOUND('',#1976,.T.);
#1415=FACE_OUTER_BOUND('',#1978,.T.);
#1416=FACE_OUTER_BOUND('',#1980,.T.);
#1417=FACE_OUTER_BOUND('',#1982,.T.);
#1418=FACE_OUTER_BOUND('',#1984,.T.);
#1419=FACE_OUTER_BOUND('',#1985,.T.);
#1420=FACE_OUTER_BOUND('',#1986,.T.);
#1421=FACE_OUTER_BOUND('',#1987,.T.);
#1422=FACE_OUTER_BOUND('',#1988,.T.);
#1423=FACE_OUTER_BOUND('',#1989,.T.);
#1424=FACE_OUTER_BOUND('',#1990,.T.);
#1425=FACE_OUTER_BOUND('',#1991,.T.);
#1426=FACE_OUTER_BOUND('',#1994,.T.);
#1427=FACE_OUTER_BOUND('',#1997,.T.);
#1428=FACE_OUTER_BOUND('',#1998,.T.);
#1429=FACE_OUTER_BOUND('',#2000,.T.);
#1430=FACE_OUTER_BOUND('',#2002,.T.);
#1431=FACE_OUTER_BOUND('',#2003,.T.);
#1432=FACE_OUTER_BOUND('',#2004,.T.);
#1433=FACE_OUTER_BOUND('',#2005,.T.);
#1434=FACE_OUTER_BOUND('',#2007,.T.);
#1435=FACE_OUTER_BOUND('',#2009,.T.);
#1436=FACE_OUTER_BOUND('',#2010,.T.);
#1437=FACE_OUTER_BOUND('',#2011,.T.);
#1438=FACE_OUTER_BOUND('',#2013,.T.);
#1439=FACE_OUTER_BOUND('',#2015,.T.);
#1440=FACE_OUTER_BOUND('',#2016,.T.);
#1441=FACE_OUTER_BOUND('',#2017,.T.);
#1442=FACE_OUTER_BOUND('',#2018,.T.);
#1443=FACE_OUTER_BOUND('',#2019,.T.);
#1444=FACE_OUTER_BOUND('',#2020,.T.);
#1445=FACE_OUTER_BOUND('',#2021,.T.);
#1446=FACE_OUTER_BOUND('',#2022,.T.);
#1447=FACE_OUTER_BOUND('',#2023,.T.);
#1448=FACE_OUTER_BOUND('',#2024,.T.);
#1449=FACE_OUTER_BOUND('',#2025,.T.);
#1450=FACE_OUTER_BOUND('',#2026,.T.);
#1451=FACE_OUTER_BOUND('',#2027,.T.);
#1452=FACE_OUTER_BOUND('',#2028,.T.);
#1453=FACE_OUTER_BOUND('',#2029,.T.);
#1454=FACE_OUTER_BOUND('',#2030,.T.);
#1455=FACE_OUTER_BOUND('',#2031,.T.);
#1456=FACE_OUTER_BOUND('',#2032,.T.);
#1457=FACE_OUTER_BOUND('',#2034,.T.);
#1458=FACE_OUTER_BOUND('',#2035,.T.);
#1459=FACE_OUTER_BOUND('',#2036,.T.);
#1460=FACE_OUTER_BOUND('',#2037,.T.);
#1461=FACE_OUTER_BOUND('',#2038,.T.);
#1462=FACE_OUTER_BOUND('',#2039,.T.);
#1463=FACE_OUTER_BOUND('',#2040,.T.);
#1464=FACE_OUTER_BOUND('',#2042,.T.);
#1465=FACE_OUTER_BOUND('',#2044,.T.);
#1466=FACE_OUTER_BOUND('',#2045,.T.);
#1467=FACE_OUTER_BOUND('',#2046,.T.);
#1468=FACE_OUTER_BOUND('',#2047,.T.);
#1469=FACE_OUTER_BOUND('',#2048,.T.);
#1470=FACE_OUTER_BOUND('',#2050,.T.);
#1471=FACE_OUTER_BOUND('',#2051,.T.);
#1472=FACE_OUTER_BOUND('',#2052,.T.);
#1473=FACE_OUTER_BOUND('',#2053,.T.);
#1474=FACE_OUTER_BOUND('',#2054,.T.);
#1475=FACE_OUTER_BOUND('',#2055,.T.);
#1476=FACE_OUTER_BOUND('',#2056,.T.);
#1477=FACE_OUTER_BOUND('',#2057,.T.);
#1478=FACE_OUTER_BOUND('',#2058,.T.);
#1479=FACE_OUTER_BOUND('',#2059,.T.);
#1480=FACE_OUTER_BOUND('',#2060,.T.);
#1481=FACE_OUTER_BOUND('',#2061,.T.);
#1482=EDGE_LOOP('',(#5159,#5160,#5161,#5162));
#1483=EDGE_LOOP('',(#5163,#5164,#5165,#5166));
#1484=EDGE_LOOP('',(#5167,#5168,#5169,#5170));
#1485=EDGE_LOOP('',(#5171,#5172,#5173,#5174));
#1486=EDGE_LOOP('',(#5175,#5176,#5177,#5178));
#1487=EDGE_LOOP('',(#5179,#5180,#5181,#5182));
#1488=EDGE_LOOP('',(#5183,#5184,#5185,#5186));
#1489=EDGE_LOOP('',(#5187,#5188,#5189,#5190));
#1490=EDGE_LOOP('',(#5191,#5192,#5193,#5194));
#1491=EDGE_LOOP('',(#5195,#5196,#5197,#5198));
#1492=EDGE_LOOP('',(#5199,#5200,#5201,#5202));
#1493=EDGE_LOOP('',(#5203,#5204,#5205,#5206));
#1494=EDGE_LOOP('',(#5207));
#1495=EDGE_LOOP('',(#5208));
#1496=EDGE_LOOP('',(#5209));
#1497=EDGE_LOOP('',(#5210));
#1498=EDGE_LOOP('',(#5211));
#1499=EDGE_LOOP('',(#5212));
#1500=EDGE_LOOP('',(#5213));
#1501=EDGE_LOOP('',(#5214,#5215,#5216,#5217));
#1502=EDGE_LOOP('',(#5218));
#1503=EDGE_LOOP('',(#5219));
#1504=EDGE_LOOP('',(#5220));
#1505=EDGE_LOOP('',(#5221));
#1506=EDGE_LOOP('',(#5222));
#1507=EDGE_LOOP('',(#5223));
#1508=EDGE_LOOP('',(#5224));
#1509=EDGE_LOOP('',(#5225,#5226,#5227,#5228));
#1510=EDGE_LOOP('',(#5229));
#1511=EDGE_LOOP('',(#5230,#5231,#5232,#5233));
#1512=EDGE_LOOP('',(#5234));
#1513=EDGE_LOOP('',(#5235,#5236,#5237,#5238));
#1514=EDGE_LOOP('',(#5239));
#1515=EDGE_LOOP('',(#5240,#5241,#5242,#5243));
#1516=EDGE_LOOP('',(#5244,#5245,#5246,#5247));
#1517=EDGE_LOOP('',(#5248,#5249,#5250,#5251));
#1518=EDGE_LOOP('',(#5252));
#1519=EDGE_LOOP('',(#5253));
#1520=EDGE_LOOP('',(#5254));
#1521=EDGE_LOOP('',(#5255,#5256,#5257,#5258));
#1522=EDGE_LOOP('',(#5259,#5260,#5261,#5262));
#1523=EDGE_LOOP('',(#5263,#5264,#5265,#5266));
#1524=EDGE_LOOP('',(#5267,#5268,#5269,#5270));
#1525=EDGE_LOOP('',(#5271));
#1526=EDGE_LOOP('',(#5272,#5273,#5274,#5275));
#1527=EDGE_LOOP('',(#5276));
#1528=EDGE_LOOP('',(#5277,#5278,#5279,#5280));
#1529=EDGE_LOOP('',(#5281));
#1530=EDGE_LOOP('',(#5282,#5283,#5284,#5285));
#1531=EDGE_LOOP('',(#5286));
#1532=EDGE_LOOP('',(#5287,#5288,#5289,#5290));
#1533=EDGE_LOOP('',(#5291,#5292,#5293,#5294));
#1534=EDGE_LOOP('',(#5295));
#1535=EDGE_LOOP('',(#5296));
#1536=EDGE_LOOP('',(#5297,#5298,#5299,#5300));
#1537=EDGE_LOOP('',(#5301,#5302,#5303,#5304));
#1538=EDGE_LOOP('',(#5305,#5306,#5307,#5308));
#1539=EDGE_LOOP('',(#5309,#5310,#5311,#5312));
#1540=EDGE_LOOP('',(#5313));
#1541=EDGE_LOOP('',(#5314));
#1542=EDGE_LOOP('',(#5315,#5316,#5317,#5318));
#1543=EDGE_LOOP('',(#5319,#5320,#5321,#5322));
#1544=EDGE_LOOP('',(#5323,#5324,#5325,#5326));
#1545=EDGE_LOOP('',(#5327,#5328,#5329,#5330));
#1546=EDGE_LOOP('',(#5331));
#1547=EDGE_LOOP('',(#5332));
#1548=EDGE_LOOP('',(#5333,#5334,#5335,#5336));
#1549=EDGE_LOOP('',(#5337,#5338,#5339,#5340));
#1550=EDGE_LOOP('',(#5341));
#1551=EDGE_LOOP('',(#5342,#5343,#5344,#5345));
#1552=EDGE_LOOP('',(#5346));
#1553=EDGE_LOOP('',(#5347,#5348,#5349,#5350));
#1554=EDGE_LOOP('',(#5351,#5352,#5353,#5354));
#1555=EDGE_LOOP('',(#5355));
#1556=EDGE_LOOP('',(#5356));
#1557=EDGE_LOOP('',(#5357));
#1558=EDGE_LOOP('',(#5358));
#1559=EDGE_LOOP('',(#5359,#5360,#5361,#5362));
#1560=EDGE_LOOP('',(#5363,#5364,#5365,#5366));
#1561=EDGE_LOOP('',(#5367));
#1562=EDGE_LOOP('',(#5368));
#1563=EDGE_LOOP('',(#5369));
#1564=EDGE_LOOP('',(#5370));
#1565=EDGE_LOOP('',(#5371,#5372,#5373,#5374));
#1566=EDGE_LOOP('',(#5375,#5376,#5377,#5378));
#1567=EDGE_LOOP('',(#5379));
#1568=EDGE_LOOP('',(#5380));
#1569=EDGE_LOOP('',(#5381,#5382,#5383,#5384));
#1570=EDGE_LOOP('',(#5385,#5386,#5387,#5388));
#1571=EDGE_LOOP('',(#5389,#5390,#5391,#5392));
#1572=EDGE_LOOP('',(#5393,#5394,#5395,#5396));
#1573=EDGE_LOOP('',(#5397,#5398));
#1574=EDGE_LOOP('',(#5399));
#1575=EDGE_LOOP('',(#5400));
#1576=EDGE_LOOP('',(#5401));
#1577=EDGE_LOOP('',(#5402));
#1578=EDGE_LOOP('',(#5403,#5404,#5405,#5406));
#1579=EDGE_LOOP('',(#5407,#5408,#5409,#5410));
#1580=EDGE_LOOP('',(#5411));
#1581=EDGE_LOOP('',(#5412));
#1582=EDGE_LOOP('',(#5413,#5414,#5415,#5416));
#1583=EDGE_LOOP('',(#5417,#5418));
#1584=EDGE_LOOP('',(#5419));
#1585=EDGE_LOOP('',(#5420));
#1586=EDGE_LOOP('',(#5421));
#1587=EDGE_LOOP('',(#5422));
#1588=EDGE_LOOP('',(#5423,#5424,#5425,#5426));
#1589=EDGE_LOOP('',(#5427,#5428,#5429,#5430));
#1590=EDGE_LOOP('',(#5431));
#1591=EDGE_LOOP('',(#5432));
#1592=EDGE_LOOP('',(#5433,#5434,#5435,#5436));
#1593=EDGE_LOOP('',(#5437,#5438,#5439,#5440));
#1594=EDGE_LOOP('',(#5441,#5442,#5443,#5444));
#1595=EDGE_LOOP('',(#5445));
#1596=EDGE_LOOP('',(#5446));
#1597=EDGE_LOOP('',(#5447,#5448,#5449,#5450));
#1598=EDGE_LOOP('',(#5451));
#1599=EDGE_LOOP('',(#5452));
#1600=EDGE_LOOP('',(#5453,#5454,#5455,#5456));
#1601=EDGE_LOOP('',(#5457));
#1602=EDGE_LOOP('',(#5458));
#1603=EDGE_LOOP('',(#5459,#5460,#5461,#5462));
#1604=EDGE_LOOP('',(#5463,#5464,#5465,#5466));
#1605=EDGE_LOOP('',(#5467,#5468,#5469,#5470));
#1606=EDGE_LOOP('',(#5471,#5472,#5473,#5474));
#1607=EDGE_LOOP('',(#5475,#5476,#5477,#5478));
#1608=EDGE_LOOP('',(#5479,#5480,#5481,#5482));
#1609=EDGE_LOOP('',(#5483,#5484,#5485,#5486));
#1610=EDGE_LOOP('',(#5487,#5488,#5489,#5490));
#1611=EDGE_LOOP('',(#5491,#5492,#5493,#5494));
#1612=EDGE_LOOP('',(#5495,#5496,#5497,#5498,#5499,#5500));
#1613=EDGE_LOOP('',(#5501,#5502,#5503,#5504,#5505,#5506));
#1614=EDGE_LOOP('',(#5507));
#1615=EDGE_LOOP('',(#5508));
#1616=EDGE_LOOP('',(#5509,#5510,#5511,#5512));
#1617=EDGE_LOOP('',(#5513,#5514,#5515,#5516));
#1618=EDGE_LOOP('',(#5517,#5518,#5519,#5520));
#1619=EDGE_LOOP('',(#5521));
#1620=EDGE_LOOP('',(#5522));
#1621=EDGE_LOOP('',(#5523,#5524,#5525,#5526));
#1622=EDGE_LOOP('',(#5527,#5528,#5529,#5530));
#1623=EDGE_LOOP('',(#5531,#5532,#5533,#5534,#5535,#5536));
#1624=EDGE_LOOP('',(#5537,#5538,#5539,#5540,#5541));
#1625=EDGE_LOOP('',(#5542,#5543,#5544,#5545));
#1626=EDGE_LOOP('',(#5546,#5547,#5548,#5549));
#1627=EDGE_LOOP('',(#5550));
#1628=EDGE_LOOP('',(#5551));
#1629=EDGE_LOOP('',(#5552,#5553,#5554,#5555,#5556));
#1630=EDGE_LOOP('',(#5557));
#1631=EDGE_LOOP('',(#5558));
#1632=EDGE_LOOP('',(#5559,#5560,#5561,#5562));
#1633=EDGE_LOOP('',(#5563,#5564,#5565,#5566,#5567,#5568));
#1634=EDGE_LOOP('',(#5569,#5570,#5571,#5572,#5573));
#1635=EDGE_LOOP('',(#5574));
#1636=EDGE_LOOP('',(#5575));
#1637=EDGE_LOOP('',(#5576,#5577,#5578,#5579));
#1638=EDGE_LOOP('',(#5580,#5581,#5582,#5583));
#1639=EDGE_LOOP('',(#5584,#5585,#5586,#5587));
#1640=EDGE_LOOP('',(#5588));
#1641=EDGE_LOOP('',(#5589));
#1642=EDGE_LOOP('',(#5590,#5591,#5592,#5593,#5594));
#1643=EDGE_LOOP('',(#5595,#5596));
#1644=EDGE_LOOP('',(#5597,#5598));
#1645=EDGE_LOOP('',(#5599,#5600));
#1646=EDGE_LOOP('',(#5601,#5602));
#1647=EDGE_LOOP('',(#5603,#5604));
#1648=EDGE_LOOP('',(#5605,#5606));
#1649=EDGE_LOOP('',(#5607,#5608));
#1650=EDGE_LOOP('',(#5609,#5610));
#1651=EDGE_LOOP('',(#5611,#5612,#5613,#5614));
#1652=EDGE_LOOP('',(#5615,#5616,#5617,#5618,#5619,#5620,#5621,#5622,#5623,
#5624,#5625,#5626,#5627,#5628,#5629,#5630,#5631,#5632,#5633,#5634));
#1653=EDGE_LOOP('',(#5635,#5636,#5637,#5638));
#1654=EDGE_LOOP('',(#5639,#5640,#5641,#5642));
#1655=EDGE_LOOP('',(#5643,#5644,#5645,#5646));
#1656=EDGE_LOOP('',(#5647,#5648,#5649,#5650));
#1657=EDGE_LOOP('',(#5651,#5652,#5653,#5654));
#1658=EDGE_LOOP('',(#5655,#5656,#5657,#5658,#5659,#5660));
#1659=EDGE_LOOP('',(#5661,#5662,#5663,#5664));
#1660=EDGE_LOOP('',(#5665,#5666,#5667,#5668));
#1661=EDGE_LOOP('',(#5669,#5670,#5671,#5672));
#1662=EDGE_LOOP('',(#5673,#5674,#5675,#5676));
#1663=EDGE_LOOP('',(#5677,#5678,#5679,#5680));
#1664=EDGE_LOOP('',(#5681,#5682,#5683,#5684));
#1665=EDGE_LOOP('',(#5685,#5686,#5687,#5688,#5689,#5690,#5691,#5692,#5693,
#5694,#5695,#5696,#5697,#5698,#5699,#5700,#5701,#5702,#5703,#5704));
#1666=EDGE_LOOP('',(#5705,#5706,#5707,#5708));
#1667=EDGE_LOOP('',(#5709,#5710,#5711,#5712));
#1668=EDGE_LOOP('',(#5713));
#1669=EDGE_LOOP('',(#5714));
#1670=EDGE_LOOP('',(#5715,#5716,#5717,#5718));
#1671=EDGE_LOOP('',(#5719));
#1672=EDGE_LOOP('',(#5720));
#1673=EDGE_LOOP('',(#5721,#5722,#5723,#5724));
#1674=EDGE_LOOP('',(#5725));
#1675=EDGE_LOOP('',(#5726));
#1676=EDGE_LOOP('',(#5727,#5728,#5729,#5730));
#1677=EDGE_LOOP('',(#5731));
#1678=EDGE_LOOP('',(#5732));
#1679=EDGE_LOOP('',(#5733,#5734,#5735,#5736));
#1680=EDGE_LOOP('',(#5737));
#1681=EDGE_LOOP('',(#5738));
#1682=EDGE_LOOP('',(#5739,#5740,#5741,#5742));
#1683=EDGE_LOOP('',(#5743,#5744,#5745,#5746));
#1684=EDGE_LOOP('',(#5747));
#1685=EDGE_LOOP('',(#5748,#5749,#5750,#5751));
#1686=EDGE_LOOP('',(#5752));
#1687=EDGE_LOOP('',(#5753,#5754,#5755,#5756));
#1688=EDGE_LOOP('',(#5757));
#1689=EDGE_LOOP('',(#5758,#5759,#5760,#5761));
#1690=EDGE_LOOP('',(#5762));
#1691=EDGE_LOOP('',(#5763,#5764,#5765,#5766));
#1692=EDGE_LOOP('',(#5767));
#1693=EDGE_LOOP('',(#5768,#5769,#5770,#5771));
#1694=EDGE_LOOP('',(#5772));
#1695=EDGE_LOOP('',(#5773));
#1696=EDGE_LOOP('',(#5774,#5775,#5776,#5777));
#1697=EDGE_LOOP('',(#5778,#5779,#5780,#5781));
#1698=EDGE_LOOP('',(#5782));
#1699=EDGE_LOOP('',(#5783));
#1700=EDGE_LOOP('',(#5784,#5785,#5786,#5787));
#1701=EDGE_LOOP('',(#5788,#5789,#5790,#5791));
#1702=EDGE_LOOP('',(#5792,#5793,#5794,#5795));
#1703=EDGE_LOOP('',(#5796));
#1704=EDGE_LOOP('',(#5797));
#1705=EDGE_LOOP('',(#5798,#5799,#5800,#5801));
#1706=EDGE_LOOP('',(#5802,#5803,#5804,#5805));
#1707=EDGE_LOOP('',(#5806,#5807,#5808,#5809,#5810,#5811,#5812,#5813));
#1708=EDGE_LOOP('',(#5814));
#1709=EDGE_LOOP('',(#5815));
#1710=EDGE_LOOP('',(#5816));
#1711=EDGE_LOOP('',(#5817));
#1712=EDGE_LOOP('',(#5818,#5819,#5820,#5821));
#1713=EDGE_LOOP('',(#5822,#5823,#5824,#5825));
#1714=EDGE_LOOP('',(#5826));
#1715=EDGE_LOOP('',(#5827));
#1716=EDGE_LOOP('',(#5828,#5829,#5830,#5831));
#1717=EDGE_LOOP('',(#5832,#5833,#5834,#5835,#5836,#5837,#5838,#5839));
#1718=EDGE_LOOP('',(#5840));
#1719=EDGE_LOOP('',(#5841));
#1720=EDGE_LOOP('',(#5842));
#1721=EDGE_LOOP('',(#5843,#5844,#5845,#5846));
#1722=EDGE_LOOP('',(#5847,#5848,#5849,#5850));
#1723=EDGE_LOOP('',(#5851,#5852,#5853,#5854));
#1724=EDGE_LOOP('',(#5855,#5856,#5857,#5858));
#1725=EDGE_LOOP('',(#5859,#5860,#5861,#5862));
#1726=EDGE_LOOP('',(#5863,#5864,#5865,#5866));
#1727=EDGE_LOOP('',(#5867,#5868,#5869,#5870));
#1728=EDGE_LOOP('',(#5871,#5872,#5873,#5874));
#1729=EDGE_LOOP('',(#5875,#5876,#5877,#5878));
#1730=EDGE_LOOP('',(#5879,#5880,#5881,#5882));
#1731=EDGE_LOOP('',(#5883));
#1732=EDGE_LOOP('',(#5884));
#1733=EDGE_LOOP('',(#5885,#5886,#5887,#5888));
#1734=EDGE_LOOP('',(#5889,#5890,#5891,#5892));
#1735=EDGE_LOOP('',(#5893,#5894,#5895,#5896));
#1736=EDGE_LOOP('',(#5897));
#1737=EDGE_LOOP('',(#5898));
#1738=EDGE_LOOP('',(#5899,#5900,#5901,#5902));
#1739=EDGE_LOOP('',(#5903));
#1740=EDGE_LOOP('',(#5904));
#1741=EDGE_LOOP('',(#5905,#5906,#5907,#5908));
#1742=EDGE_LOOP('',(#5909));
#1743=EDGE_LOOP('',(#5910));
#1744=EDGE_LOOP('',(#5911,#5912,#5913,#5914));
#1745=EDGE_LOOP('',(#5915,#5916,#5917,#5918));
#1746=EDGE_LOOP('',(#5919,#5920,#5921,#5922));
#1747=EDGE_LOOP('',(#5923,#5924,#5925,#5926));
#1748=EDGE_LOOP('',(#5927,#5928,#5929,#5930));
#1749=EDGE_LOOP('',(#5931,#5932,#5933,#5934));
#1750=EDGE_LOOP('',(#5935,#5936,#5937,#5938));
#1751=EDGE_LOOP('',(#5939,#5940,#5941,#5942));
#1752=EDGE_LOOP('',(#5943,#5944,#5945,#5946));
#1753=EDGE_LOOP('',(#5947,#5948,#5949,#5950));
#1754=EDGE_LOOP('',(#5951,#5952,#5953,#5954));
#1755=EDGE_LOOP('',(#5955,#5956,#5957));
#1756=EDGE_LOOP('',(#5958,#5959,#5960,#5961));
#1757=EDGE_LOOP('',(#5962,#5963,#5964,#5965));
#1758=EDGE_LOOP('',(#5966,#5967,#5968,#5969));
#1759=EDGE_LOOP('',(#5970,#5971,#5972,#5973));
#1760=EDGE_LOOP('',(#5974,#5975,#5976,#5977));
#1761=EDGE_LOOP('',(#5978,#5979,#5980,#5981));
#1762=EDGE_LOOP('',(#5982,#5983,#5984,#5985));
#1763=EDGE_LOOP('',(#5986,#5987,#5988,#5989));
#1764=EDGE_LOOP('',(#5990,#5991,#5992,#5993));
#1765=EDGE_LOOP('',(#5994,#5995,#5996,#5997));
#1766=EDGE_LOOP('',(#5998,#5999,#6000,#6001,#6002,#6003,#6004,#6005,#6006,
#6007,#6008,#6009,#6010,#6011,#6012,#6013,#6014,#6015,#6016,#6017,#6018,
#6019));
#1767=EDGE_LOOP('',(#6020,#6021,#6022,#6023,#6024,#6025,#6026,#6027,#6028,
#6029,#6030,#6031,#6032,#6033,#6034,#6035,#6036,#6037,#6038,#6039,#6040));
#1768=EDGE_LOOP('',(#6041,#6042));
#1769=EDGE_LOOP('',(#6043,#6044,#6045,#6046,#6047));
#1770=EDGE_LOOP('',(#6048));
#1771=EDGE_LOOP('',(#6049));
#1772=EDGE_LOOP('',(#6050));
#1773=EDGE_LOOP('',(#6051,#6052,#6053,#6054));
#1774=EDGE_LOOP('',(#6055,#6056,#6057,#6058));
#1775=EDGE_LOOP('',(#6059,#6060,#6061,#6062));
#1776=EDGE_LOOP('',(#6063,#6064,#6065,#6066));
#1777=EDGE_LOOP('',(#6067,#6068));
#1778=EDGE_LOOP('',(#6069));
#1779=EDGE_LOOP('',(#6070));
#1780=EDGE_LOOP('',(#6071));
#1781=EDGE_LOOP('',(#6072));
#1782=EDGE_LOOP('',(#6073,#6074,#6075,#6076));
#1783=EDGE_LOOP('',(#6077,#6078,#6079,#6080,#6081));
#1784=EDGE_LOOP('',(#6082,#6083,#6084,#6085));
#1785=EDGE_LOOP('',(#6086));
#1786=EDGE_LOOP('',(#6087,#6088,#6089,#6090));
#1787=EDGE_LOOP('',(#6091));
#1788=EDGE_LOOP('',(#6092,#6093,#6094,#6095));
#1789=EDGE_LOOP('',(#6096,#6097,#6098,#6099));
#1790=EDGE_LOOP('',(#6100,#6101,#6102,#6103));
#1791=EDGE_LOOP('',(#6104));
#1792=EDGE_LOOP('',(#6105));
#1793=EDGE_LOOP('',(#6106,#6107,#6108,#6109));
#1794=EDGE_LOOP('',(#6110,#6111,#6112,#6113));
#1795=EDGE_LOOP('',(#6114,#6115,#6116,#6117));
#1796=EDGE_LOOP('',(#6118));
#1797=EDGE_LOOP('',(#6119,#6120,#6121,#6122));
#1798=EDGE_LOOP('',(#6123,#6124,#6125,#6126));
#1799=EDGE_LOOP('',(#6127,#6128,#6129,#6130));
#1800=EDGE_LOOP('',(#6131,#6132,#6133,#6134));
#1801=EDGE_LOOP('',(#6135,#6136,#6137,#6138));
#1802=EDGE_LOOP('',(#6139,#6140,#6141,#6142));
#1803=EDGE_LOOP('',(#6143,#6144,#6145,#6146,#6147,#6148));
#1804=EDGE_LOOP('',(#6149,#6150,#6151,#6152,#6153,#6154));
#1805=EDGE_LOOP('',(#6155));
#1806=EDGE_LOOP('',(#6156,#6157,#6158,#6159));
#1807=EDGE_LOOP('',(#6160,#6161,#6162,#6163));
#1808=EDGE_LOOP('',(#6164,#6165,#6166,#6167));
#1809=EDGE_LOOP('',(#6168));
#1810=EDGE_LOOP('',(#6169));
#1811=EDGE_LOOP('',(#6170,#6171,#6172,#6173));
#1812=EDGE_LOOP('',(#6174,#6175,#6176,#6177));
#1813=EDGE_LOOP('',(#6178,#6179,#6180,#6181));
#1814=EDGE_LOOP('',(#6182));
#1815=EDGE_LOOP('',(#6183,#6184,#6185,#6186));
#1816=EDGE_LOOP('',(#6187,#6188,#6189,#6190));
#1817=EDGE_LOOP('',(#6191,#6192,#6193,#6194));
#1818=EDGE_LOOP('',(#6195,#6196,#6197,#6198));
#1819=EDGE_LOOP('',(#6199,#6200,#6201,#6202));
#1820=EDGE_LOOP('',(#6203,#6204,#6205,#6206));
#1821=EDGE_LOOP('',(#6207,#6208,#6209,#6210,#6211,#6212));
#1822=EDGE_LOOP('',(#6213,#6214,#6215,#6216,#6217,#6218));
#1823=EDGE_LOOP('',(#6219,#6220,#6221,#6222));
#1824=EDGE_LOOP('',(#6223,#6224,#6225,#6226));
#1825=EDGE_LOOP('',(#6227,#6228,#6229,#6230));
#1826=EDGE_LOOP('',(#6231,#6232,#6233,#6234));
#1827=EDGE_LOOP('',(#6235,#6236,#6237,#6238));
#1828=EDGE_LOOP('',(#6239,#6240,#6241,#6242));
#1829=EDGE_LOOP('',(#6243,#6244,#6245,#6246));
#1830=EDGE_LOOP('',(#6247,#6248,#6249,#6250));
#1831=EDGE_LOOP('',(#6251,#6252,#6253,#6254));
#1832=EDGE_LOOP('',(#6255,#6256,#6257,#6258));
#1833=EDGE_LOOP('',(#6259,#6260,#6261,#6262));
#1834=EDGE_LOOP('',(#6263,#6264,#6265,#6266));
#1835=EDGE_LOOP('',(#6267,#6268,#6269,#6270));
#1836=EDGE_LOOP('',(#6271,#6272,#6273,#6274));
#1837=EDGE_LOOP('',(#6275,#6276,#6277,#6278));
#1838=EDGE_LOOP('',(#6279,#6280,#6281,#6282));
#1839=EDGE_LOOP('',(#6283,#6284,#6285,#6286));
#1840=EDGE_LOOP('',(#6287,#6288,#6289,#6290));
#1841=EDGE_LOOP('',(#6291,#6292,#6293,#6294));
#1842=EDGE_LOOP('',(#6295,#6296,#6297,#6298));
#1843=EDGE_LOOP('',(#6299,#6300,#6301,#6302));
#1844=EDGE_LOOP('',(#6303,#6304,#6305,#6306));
#1845=EDGE_LOOP('',(#6307,#6308,#6309,#6310));
#1846=EDGE_LOOP('',(#6311,#6312,#6313,#6314));
#1847=EDGE_LOOP('',(#6315,#6316,#6317,#6318));
#1848=EDGE_LOOP('',(#6319,#6320,#6321,#6322));
#1849=EDGE_LOOP('',(#6323,#6324,#6325,#6326));
#1850=EDGE_LOOP('',(#6327,#6328,#6329,#6330));
#1851=EDGE_LOOP('',(#6331,#6332,#6333,#6334));
#1852=EDGE_LOOP('',(#6335,#6336,#6337,#6338));
#1853=EDGE_LOOP('',(#6339,#6340,#6341,#6342));
#1854=EDGE_LOOP('',(#6343,#6344,#6345,#6346));
#1855=EDGE_LOOP('',(#6347,#6348,#6349,#6350));
#1856=EDGE_LOOP('',(#6351,#6352,#6353,#6354));
#1857=EDGE_LOOP('',(#6355,#6356,#6357,#6358));
#1858=EDGE_LOOP('',(#6359,#6360,#6361,#6362));
#1859=EDGE_LOOP('',(#6363,#6364,#6365,#6366));
#1860=EDGE_LOOP('',(#6367,#6368,#6369,#6370));
#1861=EDGE_LOOP('',(#6371,#6372,#6373,#6374));
#1862=EDGE_LOOP('',(#6375,#6376,#6377,#6378));
#1863=EDGE_LOOP('',(#6379,#6380,#6381,#6382));
#1864=EDGE_LOOP('',(#6383,#6384,#6385,#6386));
#1865=EDGE_LOOP('',(#6387,#6388,#6389,#6390));
#1866=EDGE_LOOP('',(#6391,#6392,#6393,#6394));
#1867=EDGE_LOOP('',(#6395,#6396,#6397,#6398));
#1868=EDGE_LOOP('',(#6399,#6400,#6401,#6402));
#1869=EDGE_LOOP('',(#6403,#6404,#6405,#6406));
#1870=EDGE_LOOP('',(#6407,#6408,#6409,#6410));
#1871=EDGE_LOOP('',(#6411,#6412,#6413,#6414));
#1872=EDGE_LOOP('',(#6415,#6416,#6417,#6418));
#1873=EDGE_LOOP('',(#6419,#6420,#6421,#6422));
#1874=EDGE_LOOP('',(#6423,#6424,#6425,#6426));
#1875=EDGE_LOOP('',(#6427,#6428,#6429,#6430));
#1876=EDGE_LOOP('',(#6431,#6432,#6433,#6434));
#1877=EDGE_LOOP('',(#6435,#6436,#6437,#6438));
#1878=EDGE_LOOP('',(#6439,#6440,#6441,#6442));
#1879=EDGE_LOOP('',(#6443,#6444,#6445,#6446));
#1880=EDGE_LOOP('',(#6447,#6448,#6449,#6450));
#1881=EDGE_LOOP('',(#6451,#6452,#6453,#6454));
#1882=EDGE_LOOP('',(#6455,#6456,#6457,#6458));
#1883=EDGE_LOOP('',(#6459,#6460,#6461,#6462));
#1884=EDGE_LOOP('',(#6463,#6464,#6465,#6466));
#1885=EDGE_LOOP('',(#6467,#6468,#6469,#6470));
#1886=EDGE_LOOP('',(#6471,#6472,#6473));
#1887=EDGE_LOOP('',(#6474,#6475,#6476,#6477,#6478));
#1888=EDGE_LOOP('',(#6479,#6480,#6481,#6482));
#1889=EDGE_LOOP('',(#6483,#6484,#6485,#6486));
#1890=EDGE_LOOP('',(#6487,#6488,#6489,#6490));
#1891=EDGE_LOOP('',(#6491,#6492,#6493,#6494));
#1892=EDGE_LOOP('',(#6495,#6496,#6497,#6498));
#1893=EDGE_LOOP('',(#6499,#6500,#6501,#6502));
#1894=EDGE_LOOP('',(#6503,#6504,#6505,#6506));
#1895=EDGE_LOOP('',(#6507,#6508,#6509,#6510));
#1896=EDGE_LOOP('',(#6511,#6512,#6513,#6514));
#1897=EDGE_LOOP('',(#6515,#6516,#6517,#6518));
#1898=EDGE_LOOP('',(#6519,#6520,#6521,#6522));
#1899=EDGE_LOOP('',(#6523,#6524,#6525,#6526));
#1900=EDGE_LOOP('',(#6527,#6528,#6529,#6530));
#1901=EDGE_LOOP('',(#6531,#6532,#6533,#6534));
#1902=EDGE_LOOP('',(#6535,#6536,#6537,#6538));
#1903=EDGE_LOOP('',(#6539,#6540,#6541,#6542));
#1904=EDGE_LOOP('',(#6543,#6544,#6545,#6546));
#1905=EDGE_LOOP('',(#6547,#6548,#6549,#6550));
#1906=EDGE_LOOP('',(#6551,#6552,#6553,#6554));
#1907=EDGE_LOOP('',(#6555,#6556,#6557,#6558));
#1908=EDGE_LOOP('',(#6559,#6560,#6561,#6562));
#1909=EDGE_LOOP('',(#6563,#6564,#6565,#6566));
#1910=EDGE_LOOP('',(#6567,#6568,#6569,#6570));
#1911=EDGE_LOOP('',(#6571,#6572,#6573,#6574));
#1912=EDGE_LOOP('',(#6575,#6576,#6577,#6578));
#1913=EDGE_LOOP('',(#6579,#6580,#6581,#6582));
#1914=EDGE_LOOP('',(#6583,#6584,#6585,#6586));
#1915=EDGE_LOOP('',(#6587,#6588,#6589,#6590));
#1916=EDGE_LOOP('',(#6591,#6592,#6593,#6594));
#1917=EDGE_LOOP('',(#6595,#6596,#6597,#6598));
#1918=EDGE_LOOP('',(#6599,#6600,#6601,#6602));
#1919=EDGE_LOOP('',(#6603,#6604,#6605,#6606));
#1920=EDGE_LOOP('',(#6607,#6608,#6609,#6610));
#1921=EDGE_LOOP('',(#6611,#6612,#6613,#6614));
#1922=EDGE_LOOP('',(#6615,#6616,#6617,#6618));
#1923=EDGE_LOOP('',(#6619,#6620,#6621,#6622));
#1924=EDGE_LOOP('',(#6623,#6624,#6625,#6626));
#1925=EDGE_LOOP('',(#6627,#6628,#6629,#6630));
#1926=EDGE_LOOP('',(#6631,#6632,#6633,#6634));
#1927=EDGE_LOOP('',(#6635,#6636,#6637,#6638));
#1928=EDGE_LOOP('',(#6639,#6640,#6641,#6642));
#1929=EDGE_LOOP('',(#6643,#6644,#6645,#6646));
#1930=EDGE_LOOP('',(#6647,#6648,#6649,#6650));
#1931=EDGE_LOOP('',(#6651,#6652,#6653,#6654));
#1932=EDGE_LOOP('',(#6655,#6656,#6657,#6658));
#1933=EDGE_LOOP('',(#6659,#6660,#6661,#6662));
#1934=EDGE_LOOP('',(#6663,#6664,#6665,#6666));
#1935=EDGE_LOOP('',(#6667,#6668,#6669,#6670));
#1936=EDGE_LOOP('',(#6671,#6672,#6673,#6674));
#1937=EDGE_LOOP('',(#6675,#6676,#6677,#6678));
#1938=EDGE_LOOP('',(#6679,#6680,#6681,#6682));
#1939=EDGE_LOOP('',(#6683,#6684,#6685,#6686));
#1940=EDGE_LOOP('',(#6687,#6688,#6689,#6690));
#1941=EDGE_LOOP('',(#6691,#6692,#6693,#6694));
#1942=EDGE_LOOP('',(#6695,#6696,#6697,#6698));
#1943=EDGE_LOOP('',(#6699,#6700,#6701,#6702));
#1944=EDGE_LOOP('',(#6703,#6704,#6705,#6706));
#1945=EDGE_LOOP('',(#6707,#6708,#6709,#6710));
#1946=EDGE_LOOP('',(#6711,#6712,#6713,#6714));
#1947=EDGE_LOOP('',(#6715,#6716,#6717,#6718));
#1948=EDGE_LOOP('',(#6719,#6720,#6721,#6722));
#1949=EDGE_LOOP('',(#6723,#6724,#6725,#6726,#6727,#6728,#6729,#6730,#6731,
#6732,#6733,#6734,#6735,#6736,#6737,#6738,#6739,#6740,#6741,#6742,#6743,
#6744,#6745,#6746,#6747,#6748,#6749,#6750,#6751,#6752,#6753,#6754,#6755,
#6756,#6757,#6758,#6759,#6760,#6761,#6762,#6763,#6764,#6765,#6766,#6767,
#6768,#6769,#6770,#6771,#6772,#6773,#6774,#6775,#6776,#6777,#6778,#6779,
#6780,#6781,#6782,#6783,#6784,#6785,#6786,#6787,#6788,#6789,#6790,#6791,
#6792,#6793,#6794,#6795,#6796,#6797,#6798,#6799,#6800,#6801,#6802,#6803,
#6804,#6805,#6806,#6807,#6808,#6809,#6810,#6811,#6812,#6813,#6814,#6815,
#6816,#6817,#6818,#6819,#6820,#6821,#6822,#6823,#6824,#6825,#6826,#6827,
#6828,#6829,#6830,#6831,#6832,#6833,#6834,#6835,#6836,#6837,#6838,#6839,
#6840,#6841,#6842,#6843,#6844,#6845,#6846,#6847,#6848,#6849,#6850,#6851));
#1950=EDGE_LOOP('',(#6852,#6853,#6854,#6855));
#1951=EDGE_LOOP('',(#6856,#6857,#6858,#6859,#6860,#6861,#6862,#6863,#6864,
#6865,#6866,#6867,#6868,#6869,#6870,#6871,#6872,#6873,#6874,#6875,#6876,
#6877,#6878,#6879,#6880,#6881,#6882,#6883,#6884,#6885,#6886,#6887,#6888,
#6889,#6890,#6891,#6892,#6893,#6894,#6895,#6896,#6897,#6898,#6899,#6900,
#6901,#6902,#6903,#6904,#6905,#6906,#6907,#6908,#6909,#6910,#6911,#6912,
#6913,#6914,#6915,#6916,#6917,#6918,#6919,#6920,#6921,#6922,#6923,#6924,
#6925,#6926,#6927,#6928,#6929,#6930,#6931,#6932,#6933,#6934,#6935,#6936,
#6937,#6938,#6939,#6940,#6941,#6942,#6943,#6944,#6945,#6946,#6947,#6948,
#6949,#6950,#6951,#6952,#6953,#6954,#6955,#6956,#6957,#6958,#6959,#6960,
#6961,#6962,#6963,#6964,#6965,#6966,#6967,#6968,#6969,#6970,#6971,#6972,
#6973,#6974,#6975,#6976,#6977,#6978,#6979,#6980,#6981,#6982,#6983,#6984,
#6985));
#1952=EDGE_LOOP('',(#6986,#6987,#6988,#6989));
#1953=EDGE_LOOP('',(#6990,#6991,#6992,#6993));
#1954=EDGE_LOOP('',(#6994,#6995,#6996,#6997));
#1955=EDGE_LOOP('',(#6998,#6999,#7000,#7001));
#1956=EDGE_LOOP('',(#7002,#7003,#7004,#7005));
#1957=EDGE_LOOP('',(#7006,#7007,#7008,#7009));
#1958=EDGE_LOOP('',(#7010,#7011,#7012,#7013));
#1959=EDGE_LOOP('',(#7014));
#1960=EDGE_LOOP('',(#7015));
#1961=EDGE_LOOP('',(#7016,#7017,#7018,#7019,#7020));
#1962=EDGE_LOOP('',(#7021,#7022,#7023,#7024));
#1963=EDGE_LOOP('',(#7025));
#1964=EDGE_LOOP('',(#7026));
#1965=EDGE_LOOP('',(#7027,#7028,#7029,#7030));
#1966=EDGE_LOOP('',(#7031,#7032,#7033,#7034));
#1967=EDGE_LOOP('',(#7035,#7036,#7037,#7038));
#1968=EDGE_LOOP('',(#7039,#7040,#7041,#7042));
#1969=EDGE_LOOP('',(#7043));
#1970=EDGE_LOOP('',(#7044));
#1971=EDGE_LOOP('',(#7045));
#1972=EDGE_LOOP('',(#7046));
#1973=EDGE_LOOP('',(#7047,#7048));
#1974=EDGE_LOOP('',(#7049,#7050,#7051,#7052,#7053,#7054,#7055,#7056,#7057));
#1975=EDGE_LOOP('',(#7058,#7059));
#1976=EDGE_LOOP('',(#7060,#7061,#7062,#7063));
#1977=EDGE_LOOP('',(#7064,#7065,#7066,#7067,#7068));
#1978=EDGE_LOOP('',(#7069,#7070,#7071,#7072));
#1979=EDGE_LOOP('',(#7073,#7074));
#1980=EDGE_LOOP('',(#7075));
#1981=EDGE_LOOP('',(#7076));
#1982=EDGE_LOOP('',(#7077));
#1983=EDGE_LOOP('',(#7078));
#1984=EDGE_LOOP('',(#7079,#7080,#7081,#7082));
#1985=EDGE_LOOP('',(#7083,#7084));
#1986=EDGE_LOOP('',(#7085,#7086,#7087,#7088,#7089,#7090,#7091,#7092,#7093));
#1987=EDGE_LOOP('',(#7094,#7095));
#1988=EDGE_LOOP('',(#7096,#7097,#7098,#7099,#7100,#7101));
#1989=EDGE_LOOP('',(#7102,#7103,#7104,#7105));
#1990=EDGE_LOOP('',(#7106,#7107,#7108,#7109,#7110,#7111));
#1991=EDGE_LOOP('',(#7112));
#1992=EDGE_LOOP('',(#7113));
#1993=EDGE_LOOP('',(#7114,#7115,#7116,#7117));
#1994=EDGE_LOOP('',(#7118));
#1995=EDGE_LOOP('',(#7119));
#1996=EDGE_LOOP('',(#7120,#7121,#7122,#7123));
#1997=EDGE_LOOP('',(#7124,#7125,#7126,#7127));
#1998=EDGE_LOOP('',(#7128,#7129,#7130,#7131));
#1999=EDGE_LOOP('',(#7132,#7133,#7134,#7135,#7136));
#2000=EDGE_LOOP('',(#7137,#7138,#7139,#7140));
#2001=EDGE_LOOP('',(#7141,#7142));
#2002=EDGE_LOOP('',(#7143,#7144,#7145,#7146));
#2003=EDGE_LOOP('',(#7147,#7148,#7149,#7150));
#2004=EDGE_LOOP('',(#7151,#7152,#7153,#7154));
#2005=EDGE_LOOP('',(#7155));
#2006=EDGE_LOOP('',(#7156));
#2007=EDGE_LOOP('',(#7157));
#2008=EDGE_LOOP('',(#7158));
#2009=EDGE_LOOP('',(#7159,#7160,#7161,#7162));
#2010=EDGE_LOOP('',(#7163,#7164,#7165,#7166));
#2011=EDGE_LOOP('',(#7167));
#2012=EDGE_LOOP('',(#7168));
#2013=EDGE_LOOP('',(#7169));
#2014=EDGE_LOOP('',(#7170));
#2015=EDGE_LOOP('',(#7171,#7172,#7173,#7174,#7175,#7176,#7177,#7178));
#2016=EDGE_LOOP('',(#7179,#7180,#7181,#7182));
#2017=EDGE_LOOP('',(#7183,#7184,#7185,#7186));
#2018=EDGE_LOOP('',(#7187,#7188,#7189,#7190));
#2019=EDGE_LOOP('',(#7191,#7192,#7193,#7194));
#2020=EDGE_LOOP('',(#7195,#7196,#7197,#7198,#7199,#7200,#7201,#7202));
#2021=EDGE_LOOP('',(#7203,#7204,#7205,#7206));
#2022=EDGE_LOOP('',(#7207,#7208,#7209,#7210));
#2023=EDGE_LOOP('',(#7211,#7212,#7213,#7214));
#2024=EDGE_LOOP('',(#7215,#7216,#7217,#7218));
#2025=EDGE_LOOP('',(#7219,#7220,#7221,#7222));
#2026=EDGE_LOOP('',(#7223,#7224,#7225,#7226));
#2027=EDGE_LOOP('',(#7227,#7228,#7229,#7230));
#2028=EDGE_LOOP('',(#7231,#7232,#7233,#7234));
#2029=EDGE_LOOP('',(#7235,#7236,#7237,#7238));
#2030=EDGE_LOOP('',(#7239,#7240,#7241,#7242));
#2031=EDGE_LOOP('',(#7243,#7244,#7245,#7246,#7247,#7248));
#2032=EDGE_LOOP('',(#7249));
#2033=EDGE_LOOP('',(#7250,#7251,#7252,#7253,#7254,#7255));
#2034=EDGE_LOOP('',(#7256,#7257,#7258,#7259));
#2035=EDGE_LOOP('',(#7260,#7261,#7262,#7263));
#2036=EDGE_LOOP('',(#7264,#7265,#7266,#7267));
#2037=EDGE_LOOP('',(#7268));
#2038=EDGE_LOOP('',(#7269,#7270,#7271,#7272));
#2039=EDGE_LOOP('',(#7273,#7274,#7275,#7276));
#2040=EDGE_LOOP('',(#7277));
#2041=EDGE_LOOP('',(#7278));
#2042=EDGE_LOOP('',(#7279));
#2043=EDGE_LOOP('',(#7280));
#2044=EDGE_LOOP('',(#7281));
#2045=EDGE_LOOP('',(#7282,#7283,#7284,#7285));
#2046=EDGE_LOOP('',(#7286,#7287,#7288,#7289));
#2047=EDGE_LOOP('',(#7290,#7291,#7292,#7293));
#2048=EDGE_LOOP('',(#7294));
#2049=EDGE_LOOP('',(#7295));
#2050=EDGE_LOOP('',(#7296,#7297,#7298,#7299));
#2051=EDGE_LOOP('',(#7300,#7301,#7302,#7303));
#2052=EDGE_LOOP('',(#7304,#7305,#7306,#7307));
#2053=EDGE_LOOP('',(#7308));
#2054=EDGE_LOOP('',(#7309,#7310,#7311,#7312));
#2055=EDGE_LOOP('',(#7313,#7314,#7315,#7316));
#2056=EDGE_LOOP('',(#7317,#7318,#7319,#7320));
#2057=EDGE_LOOP('',(#7321,#7322,#7323,#7324));
#2058=EDGE_LOOP('',(#7325,#7326,#7327,#7328));
#2059=EDGE_LOOP('',(#7329,#7330,#7331,#7332));
#2060=EDGE_LOOP('',(#7333,#7334,#7335,#7336,#7337,#7338));
#2061=EDGE_LOOP('',(#7339,#7340,#7341,#7342,#7343,#7344));
#2062=LINE('',#11325,#2570);
#2063=LINE('',#11331,#2571);
#2064=LINE('',#11337,#2572);
#2065=LINE('',#11343,#2573);
#2066=LINE('',#11349,#2574);
#2067=LINE('',#11355,#2575);
#2068=LINE('',#11361,#2576);
#2069=LINE('',#11366,#2577);
#2070=LINE('',#11368,#2578);
#2071=LINE('',#11370,#2579);
#2072=LINE('',#11371,#2580);
#2073=LINE('',#11374,#2581);
#2074=LINE('',#11376,#2582);
#2075=LINE('',#11377,#2583);
#2076=LINE('',#11380,#2584);
#2077=LINE('',#11382,#2585);
#2078=LINE('',#11383,#2586);
#2079=LINE('',#11385,#2587);
#2080=LINE('',#11386,#2588);
#2081=LINE('',#11394,#2589);
#2082=LINE('',#11401,#2590);
#2083=LINE('',#11408,#2591);
#2084=LINE('',#11414,#2592);
#2085=LINE('',#11416,#2593);
#2086=LINE('',#11418,#2594);
#2087=LINE('',#11419,#2595);
#2088=LINE('',#11422,#2596);
#2089=LINE('',#11424,#2597);
#2090=LINE('',#11425,#2598);
#2091=LINE('',#11428,#2599);
#2092=LINE('',#11430,#2600);
#2093=LINE('',#11431,#2601);
#2094=LINE('',#11433,#2602);
#2095=LINE('',#11434,#2603);
#2096=LINE('',#11442,#2604);
#2097=LINE('',#11449,#2605);
#2098=LINE('',#11456,#2606);
#2099=LINE('',#11463,#2607);
#2100=LINE('',#11469,#2608);
#2101=LINE('',#11471,#2609);
#2102=LINE('',#11473,#2610);
#2103=LINE('',#11474,#2611);
#2104=LINE('',#11477,#2612);
#2105=LINE('',#11479,#2613);
#2106=LINE('',#11480,#2614);
#2107=LINE('',#11483,#2615);
#2108=LINE('',#11485,#2616);
#2109=LINE('',#11486,#2617);
#2110=LINE('',#11488,#2618);
#2111=LINE('',#11489,#2619);
#2112=LINE('',#11497,#2620);
#2113=LINE('',#11503,#2621);
#2114=LINE('',#11509,#2622);
#2115=LINE('',#11515,#2623);
#2116=LINE('',#11523,#2624);
#2117=LINE('',#11528,#2625);
#2118=LINE('',#11535,#2626);
#2119=LINE('',#11541,#2627);
#2120=LINE('',#11543,#2628);
#2121=LINE('',#11545,#2629);
#2122=LINE('',#11546,#2630);
#2123=LINE('',#11549,#2631);
#2124=LINE('',#11551,#2632);
#2125=LINE('',#11552,#2633);
#2126=LINE('',#11555,#2634);
#2127=LINE('',#11557,#2635);
#2128=LINE('',#11558,#2636);
#2129=LINE('',#11560,#2637);
#2130=LINE('',#11561,#2638);
#2131=LINE('',#11569,#2639);
#2132=LINE('',#11575,#2640);
#2133=LINE('',#11581,#2641);
#2134=LINE('',#11586,#2642);
#2135=LINE('',#11588,#2643);
#2136=LINE('',#11590,#2644);
#2137=LINE('',#11591,#2645);
#2138=LINE('',#11600,#2646);
#2139=LINE('',#11608,#2647);
#2140=LINE('',#11614,#2648);
#2141=LINE('',#11616,#2649);
#2142=LINE('',#11618,#2650);
#2143=LINE('',#11619,#2651);
#2144=LINE('',#11622,#2652);
#2145=LINE('',#11624,#2653);
#2146=LINE('',#11625,#2654);
#2147=LINE('',#11632,#2655);
#2148=LINE('',#11633,#2656);
#2149=LINE('',#11636,#2657);
#2150=LINE('',#11637,#2658);
#2151=LINE('',#11639,#2659);
#2152=LINE('',#11647,#2660);
#2153=LINE('',#11654,#2661);
#2154=LINE('',#11659,#2662);
#2155=LINE('',#11661,#2663);
#2156=LINE('',#11667,#2664);
#2157=LINE('',#11669,#2665);
#2158=LINE('',#11671,#2666);
#2159=LINE('',#11672,#2667);
#2160=LINE('',#11675,#2668);
#2161=LINE('',#11677,#2669);
#2162=LINE('',#11678,#2670);
#2163=LINE('',#11681,#2671);
#2164=LINE('',#11683,#2672);
#2165=LINE('',#11684,#2673);
#2166=LINE('',#11687,#2674);
#2167=LINE('',#11689,#2675);
#2168=LINE('',#11690,#2676);
#2169=LINE('',#11693,#2677);
#2170=LINE('',#11695,#2678);
#2171=LINE('',#11696,#2679);
#2172=LINE('',#11698,#2680);
#2173=LINE('',#11699,#2681);
#2174=LINE('',#11711,#2682);
#2175=LINE('',#11715,#2683);
#2176=LINE('',#11719,#2684);
#2177=LINE('',#11726,#2685);
#2178=LINE('',#11728,#2686);
#2179=LINE('',#11743,#2687);
#2180=LINE('',#11749,#2688);
#2181=LINE('',#11753,#2689);
#2182=LINE('',#11759,#2690);
#2183=LINE('',#11764,#2691);
#2184=LINE('',#11779,#2692);
#2185=LINE('',#11788,#2693);
#2186=LINE('',#11792,#2694);
#2187=LINE('',#11796,#2695);
#2188=LINE('',#11799,#2696);
#2189=LINE('',#11952,#2697);
#2190=LINE('',#12248,#2698);
#2191=LINE('',#12290,#2699);
#2192=LINE('',#12295,#2700);
#2193=LINE('',#12304,#2701);
#2194=LINE('',#12309,#2702);
#2195=LINE('',#12321,#2703);
#2196=LINE('',#12328,#2704);
#2197=LINE('',#12335,#2705);
#2198=LINE('',#12342,#2706);
#2199=LINE('',#12349,#2707);
#2200=LINE('',#12356,#2708);
#2201=LINE('',#12364,#2709);
#2202=LINE('',#12369,#2710);
#2203=LINE('',#12377,#2711);
#2204=LINE('',#12382,#2712);
#2205=LINE('',#12387,#2713);
#2206=LINE('',#12389,#2714);
#2207=LINE('',#12391,#2715);
#2208=LINE('',#12392,#2716);
#2209=LINE('',#12395,#2717);
#2210=LINE('',#12397,#2718);
#2211=LINE('',#12398,#2719);
#2212=LINE('',#12401,#2720);
#2213=LINE('',#12403,#2721);
#2214=LINE('',#12404,#2722);
#2215=LINE('',#12407,#2723);
#2216=LINE('',#12409,#2724);
#2217=LINE('',#12411,#2725);
#2218=LINE('',#12413,#2726);
#2219=LINE('',#12414,#2727);
#2220=LINE('',#12417,#2728);
#2221=LINE('',#12418,#2729);
#2222=LINE('',#12421,#2730);
#2223=LINE('',#12422,#2731);
#2224=LINE('',#12425,#2732);
#2225=LINE('',#12427,#2733);
#2226=LINE('',#12428,#2734);
#2227=LINE('',#12430,#2735);
#2228=LINE('',#12431,#2736);
#2229=LINE('',#12438,#2737);
#2230=LINE('',#12440,#2738);
#2231=LINE('',#12442,#2739);
#2232=LINE('',#12443,#2740);
#2233=LINE('',#12446,#2741);
#2234=LINE('',#12448,#2742);
#2235=LINE('',#12449,#2743);
#2236=LINE('',#12452,#2744);
#2237=LINE('',#12454,#2745);
#2238=LINE('',#12455,#2746);
#2239=LINE('',#12457,#2747);
#2240=LINE('',#12458,#2748);
#2241=LINE('',#12465,#2749);
#2242=LINE('',#12467,#2750);
#2243=LINE('',#12469,#2751);
#2244=LINE('',#12470,#2752);
#2245=LINE('',#12473,#2753);
#2246=LINE('',#12475,#2754);
#2247=LINE('',#12476,#2755);
#2248=LINE('',#12483,#2756);
#2249=LINE('',#12484,#2757);
#2250=LINE('',#12487,#2758);
#2251=LINE('',#12488,#2759);
#2252=LINE('',#12490,#2760);
#2253=LINE('',#12497,#2761);
#2254=LINE('',#12504,#2762);
#2255=LINE('',#12510,#2763);
#2256=LINE('',#12512,#2764);
#2257=LINE('',#12518,#2765);
#2258=LINE('',#12590,#2766);
#2259=LINE('',#12677,#2767);
#2260=LINE('',#12767,#2768);
#2261=LINE('',#12854,#2769);
#2262=LINE('',#12944,#2770);
#2263=LINE('',#13031,#2771);
#2264=LINE('',#13118,#2772);
#2265=LINE('',#13208,#2773);
#2266=LINE('',#13224,#2774);
#2267=LINE('',#13250,#2775);
#2268=LINE('',#13287,#2776);
#2269=LINE('',#13324,#2777);
#2270=LINE('',#13362,#2778);
#2271=LINE('',#13399,#2779);
#2272=LINE('',#13436,#2780);
#2273=LINE('',#13474,#2781);
#2274=LINE('',#13512,#2782);
#2275=LINE('',#14677,#2783);
#2276=LINE('',#14689,#2784);
#2277=LINE('',#14693,#2785);
#2278=LINE('',#14697,#2786);
#2279=LINE('',#14701,#2787);
#2280=LINE('',#14702,#2788);
#2281=LINE('',#14703,#2789);
#2282=LINE('',#14712,#2790);
#2283=LINE('',#14722,#2791);
#2284=LINE('',#14726,#2792);
#2285=LINE('',#14730,#2793);
#2286=LINE('',#14737,#2794);
#2287=LINE('',#14741,#2795);
#2288=LINE('',#14745,#2796);
#2289=LINE('',#14750,#2797);
#2290=LINE('',#14752,#2798);
#2291=LINE('',#14754,#2799);
#2292=LINE('',#14755,#2800);
#2293=LINE('',#14758,#2801);
#2294=LINE('',#14760,#2802);
#2295=LINE('',#14761,#2803);
#2296=LINE('',#14764,#2804);
#2297=LINE('',#14766,#2805);
#2298=LINE('',#14767,#2806);
#2299=LINE('',#14770,#2807);
#2300=LINE('',#14772,#2808);
#2301=LINE('',#14773,#2809);
#2302=LINE('',#14776,#2810);
#2303=LINE('',#14778,#2811);
#2304=LINE('',#14779,#2812);
#2305=LINE('',#14781,#2813);
#2306=LINE('',#14782,#2814);
#2307=LINE('',#14792,#2815);
#2308=LINE('',#14796,#2816);
#2309=LINE('',#14800,#2817);
#2310=LINE('',#14807,#2818);
#2311=LINE('',#14811,#2819);
#2312=LINE('',#14815,#2820);
#2313=LINE('',#14820,#2821);
#2314=LINE('',#14822,#2822);
#2315=LINE('',#14824,#2823);
#2316=LINE('',#14825,#2824);
#2317=LINE('',#14828,#2825);
#2318=LINE('',#14830,#2826);
#2319=LINE('',#14831,#2827);
#2320=LINE('',#14834,#2828);
#2321=LINE('',#14836,#2829);
#2322=LINE('',#14837,#2830);
#2323=LINE('',#14840,#2831);
#2324=LINE('',#14842,#2832);
#2325=LINE('',#14843,#2833);
#2326=LINE('',#14846,#2834);
#2327=LINE('',#14848,#2835);
#2328=LINE('',#14849,#2836);
#2329=LINE('',#14851,#2837);
#2330=LINE('',#14852,#2838);
#2331=LINE('',#14871,#2839);
#2332=LINE('',#14901,#2840);
#2333=LINE('',#14988,#2841);
#2334=LINE('',#15078,#2842);
#2335=LINE('',#15165,#2843);
#2336=LINE('',#15252,#2844);
#2337=LINE('',#15339,#2845);
#2338=LINE('',#15426,#2846);
#2339=LINE('',#15513,#2847);
#2340=LINE('',#15585,#2848);
#2341=LINE('',#15636,#2849);
#2342=LINE('',#15684,#2850);
#2343=LINE('',#15732,#2851);
#2344=LINE('',#15783,#2852);
#2345=LINE('',#15834,#2853);
#2346=LINE('',#15882,#2854);
#2347=LINE('',#15933,#2855);
#2348=LINE('',#15984,#2856);
#2349=LINE('',#16032,#2857);
#2350=LINE('',#16080,#2858);
#2351=LINE('',#16131,#2859);
#2352=LINE('',#16182,#2860);
#2353=LINE('',#16230,#2861);
#2354=LINE('',#16281,#2862);
#2355=LINE('',#16332,#2863);
#2356=LINE('',#16380,#2864);
#2357=LINE('',#16428,#2865);
#2358=LINE('',#16479,#2866);
#2359=LINE('',#16530,#2867);
#2360=LINE('',#16578,#2868);
#2361=LINE('',#16629,#2869);
#2362=LINE('',#16680,#2870);
#2363=LINE('',#16728,#2871);
#2364=LINE('',#16776,#2872);
#2365=LINE('',#16827,#2873);
#2366=LINE('',#16878,#2874);
#2367=LINE('',#16926,#2875);
#2368=LINE('',#16977,#2876);
#2369=LINE('',#17028,#2877);
#2370=LINE('',#17076,#2878);
#2371=LINE('',#17124,#2879);
#2372=LINE('',#17175,#2880);
#2373=LINE('',#17226,#2881);
#2374=LINE('',#17274,#2882);
#2375=LINE('',#17325,#2883);
#2376=LINE('',#17376,#2884);
#2377=LINE('',#17424,#2885);
#2378=LINE('',#17472,#2886);
#2379=LINE('',#17523,#2887);
#2380=LINE('',#17574,#2888);
#2381=LINE('',#17622,#2889);
#2382=LINE('',#17673,#2890);
#2383=LINE('',#17724,#2891);
#2384=LINE('',#17772,#2892);
#2385=LINE('',#17820,#2893);
#2386=LINE('',#17871,#2894);
#2387=LINE('',#17937,#2895);
#2388=LINE('',#18027,#2896);
#2389=LINE('',#18114,#2897);
#2390=LINE('',#18201,#2898);
#2391=LINE('',#18288,#2899);
#2392=LINE('',#18375,#2900);
#2393=LINE('',#18462,#2901);
#2394=LINE('',#18552,#2902);
#2395=LINE('',#18562,#2903);
#2396=LINE('',#18598,#2904);
#2397=LINE('',#18636,#2905);
#2398=LINE('',#18672,#2906);
#2399=LINE('',#18710,#2907);
#2400=LINE('',#18746,#2908);
#2401=LINE('',#18784,#2909);
#2402=LINE('',#18821,#2910);
#2403=LINE('',#18856,#2911);
#2404=LINE('',#18883,#2912);
#2405=LINE('',#18907,#2913);
#2406=LINE('',#18931,#2914);
#2407=LINE('',#18955,#2915);
#2408=LINE('',#18981,#2916);
#2409=LINE('',#19005,#2917);
#2410=LINE('',#19029,#2918);
#2411=LINE('',#19055,#2919);
#2412=LINE('',#19079,#2920);
#2413=LINE('',#19103,#2921);
#2414=LINE('',#19127,#2922);
#2415=LINE('',#19153,#2923);
#2416=LINE('',#19177,#2924);
#2417=LINE('',#19201,#2925);
#2418=LINE('',#19227,#2926);
#2419=LINE('',#19251,#2927);
#2420=LINE('',#19275,#2928);
#2421=LINE('',#19299,#2929);
#2422=LINE('',#19325,#2930);
#2423=LINE('',#19349,#2931);
#2424=LINE('',#19373,#2932);
#2425=LINE('',#19399,#2933);
#2426=LINE('',#19423,#2934);
#2427=LINE('',#19447,#2935);
#2428=LINE('',#19471,#2936);
#2429=LINE('',#19497,#2937);
#2430=LINE('',#19521,#2938);
#2431=LINE('',#19545,#2939);
#2432=LINE('',#19571,#2940);
#2433=LINE('',#19595,#2941);
#2434=LINE('',#19619,#2942);
#2435=LINE('',#19643,#2943);
#2436=LINE('',#19669,#2944);
#2437=LINE('',#19693,#2945);
#2438=LINE('',#19717,#2946);
#2439=LINE('',#19743,#2947);
#2440=LINE('',#19767,#2948);
#2441=LINE('',#19791,#2949);
#2442=LINE('',#19815,#2950);
#2443=LINE('',#19841,#2951);
#2444=LINE('',#19865,#2952);
#2445=LINE('',#19889,#2953);
#2446=LINE('',#19915,#2954);
#2447=LINE('',#19939,#2955);
#2448=LINE('',#19963,#2956);
#2449=LINE('',#19988,#2957);
#2450=LINE('',#20015,#2958);
#2451=LINE('',#20052,#2959);
#2452=LINE('',#20088,#2960);
#2453=LINE('',#20126,#2961);
#2454=LINE('',#20162,#2962);
#2455=LINE('',#20200,#2963);
#2456=LINE('',#20237,#2964);
#2457=LINE('',#24479,#2965);
#2458=LINE('',#24481,#2966);
#2459=LINE('',#24483,#2967);
#2460=LINE('',#24484,#2968);
#2461=LINE('',#24489,#2969);
#2462=LINE('',#24490,#2970);
#2463=LINE('',#24493,#2971);
#2464=LINE('',#24494,#2972);
#2465=LINE('',#24497,#2973);
#2466=LINE('',#24498,#2974);
#2467=LINE('',#24505,#2975);
#2468=LINE('',#24515,#2976);
#2469=LINE('',#24524,#2977);
#2470=LINE('',#24530,#2978);
#2471=LINE('',#24538,#2979);
#2472=LINE('',#24576,#2980);
#2473=LINE('',#24615,#2981);
#2474=LINE('',#24620,#2982);
#2475=LINE('',#24626,#2983);
#2476=LINE('',#24635,#2984);
#2477=LINE('',#24640,#2985);
#2478=LINE('',#24670,#2986);
#2479=LINE('',#24709,#2987);
#2480=LINE('',#24713,#2988);
#2481=LINE('',#24715,#2989);
#2482=LINE('',#24717,#2990);
#2483=LINE('',#24719,#2991);
#2484=LINE('',#24721,#2992);
#2485=LINE('',#24722,#2993);
#2486=LINE('',#24725,#2994);
#2487=LINE('',#24727,#2995);
#2488=LINE('',#24728,#2996);
#2489=LINE('',#24731,#2997);
#2490=LINE('',#24733,#2998);
#2491=LINE('',#24735,#2999);
#2492=LINE('',#24737,#3000);
#2493=LINE('',#24738,#3001);
#2494=LINE('',#24748,#3002);
#2495=LINE('',#24759,#3003);
#2496=LINE('',#24765,#3004);
#2497=LINE('',#24774,#3005);
#2498=LINE('',#24780,#3006);
#2499=LINE('',#24788,#3007);
#2500=LINE('',#24790,#3008);
#2501=LINE('',#24792,#3009);
#2502=LINE('',#24794,#3010);
#2503=LINE('',#24796,#3011);
#2504=LINE('',#24798,#3012);
#2505=LINE('',#24800,#3013);
#2506=LINE('',#24801,#3014);
#2507=LINE('',#24804,#3015);
#2508=LINE('',#24806,#3016);
#2509=LINE('',#24807,#3017);
#2510=LINE('',#24810,#3018);
#2511=LINE('',#24811,#3019);
#2512=LINE('',#24814,#3020);
#2513=LINE('',#24815,#3021);
#2514=LINE('',#24818,#3022);
#2515=LINE('',#24819,#3023);
#2516=LINE('',#24823,#3024);
#2517=LINE('',#24824,#3025);
#2518=LINE('',#24826,#3026);
#2519=LINE('',#24827,#3027);
#2520=LINE('',#24829,#3028);
#2521=LINE('',#24831,#3029);
#2522=LINE('',#24833,#3030);
#2523=LINE('',#24839,#3031);
#2524=LINE('',#24841,#3032);
#2525=LINE('',#24843,#3033);
#2526=LINE('',#24844,#3034);
#2527=LINE('',#24847,#3035);
#2528=LINE('',#24849,#3036);
#2529=LINE('',#24850,#3037);
#2530=LINE('',#24853,#3038);
#2531=LINE('',#24855,#3039);
#2532=LINE('',#24856,#3040);
#2533=LINE('',#24859,#3041);
#2534=LINE('',#24861,#3042);
#2535=LINE('',#24862,#3043);
#2536=LINE('',#24865,#3044);
#2537=LINE('',#24867,#3045);
#2538=LINE('',#24868,#3046);
#2539=LINE('',#24870,#3047);
#2540=LINE('',#24871,#3048);
#2541=LINE('',#24879,#3049);
#2542=LINE('',#24883,#3050);
#2543=LINE('',#24887,#3051);
#2544=LINE('',#24894,#3052);
#2545=LINE('',#24900,#3053);
#2546=LINE('',#24911,#3054);
#2547=LINE('',#24915,#3055);
#2548=LINE('',#24919,#3056);
#2549=LINE('',#24926,#3057);
#2550=LINE('',#24930,#3058);
#2551=LINE('',#24934,#3059);
#2552=LINE('',#24939,#3060);
#2553=LINE('',#24941,#3061);
#2554=LINE('',#24943,#3062);
#2555=LINE('',#24944,#3063);
#2556=LINE('',#24947,#3064);
#2557=LINE('',#24949,#3065);
#2558=LINE('',#24950,#3066);
#2559=LINE('',#24953,#3067);
#2560=LINE('',#24955,#3068);
#2561=LINE('',#24956,#3069);
#2562=LINE('',#24959,#3070);
#2563=LINE('',#24961,#3071);
#2564=LINE('',#24962,#3072);
#2565=LINE('',#24965,#3073);
#2566=LINE('',#24967,#3074);
#2567=LINE('',#24968,#3075);
#2568=LINE('',#24970,#3076);
#2569=LINE('',#24971,#3077);
#2570=VECTOR('',#9214,0.33);
#2571=VECTOR('',#9221,0.33);
#2572=VECTOR('',#9228,0.329999999999998);
#2573=VECTOR('',#9235,0.33);
#2574=VECTOR('',#9242,0.329999999999998);
#2575=VECTOR('',#9249,0.33);
#2576=VECTOR('',#9256,0.329999999999998);
#2577=VECTOR('',#9261,1.);
#2578=VECTOR('',#9262,1.);
#2579=VECTOR('',#9263,1.);
#2580=VECTOR('',#9264,1.);
#2581=VECTOR('',#9267,1.);
#2582=VECTOR('',#9268,1.);
#2583=VECTOR('',#9269,1.);
#2584=VECTOR('',#9272,1.);
#2585=VECTOR('',#9273,1.);
#2586=VECTOR('',#9274,1.);
#2587=VECTOR('',#9277,1.);
#2588=VECTOR('',#9278,1.);
#2589=VECTOR('',#9289,0.25);
#2590=VECTOR('',#9298,0.25);
#2591=VECTOR('',#9307,0.25);
#2592=VECTOR('',#9314,1.);
#2593=VECTOR('',#9315,1.);
#2594=VECTOR('',#9316,1.);
#2595=VECTOR('',#9317,1.);
#2596=VECTOR('',#9320,1.);
#2597=VECTOR('',#9321,1.);
#2598=VECTOR('',#9322,1.);
#2599=VECTOR('',#9325,1.);
#2600=VECTOR('',#9326,1.);
#2601=VECTOR('',#9327,1.);
#2602=VECTOR('',#9330,1.);
#2603=VECTOR('',#9331,1.);
#2604=VECTOR('',#9342,0.21);
#2605=VECTOR('',#9351,0.21);
#2606=VECTOR('',#9360,0.25);
#2607=VECTOR('',#9369,0.25);
#2608=VECTOR('',#9376,1.);
#2609=VECTOR('',#9377,1.);
#2610=VECTOR('',#9378,1.);
#2611=VECTOR('',#9379,1.);
#2612=VECTOR('',#9382,1.);
#2613=VECTOR('',#9383,1.);
#2614=VECTOR('',#9384,1.);
#2615=VECTOR('',#9387,1.);
#2616=VECTOR('',#9388,1.);
#2617=VECTOR('',#9389,1.);
#2618=VECTOR('',#9392,1.);
#2619=VECTOR('',#9393,1.);
#2620=VECTOR('',#9404,0.165);
#2621=VECTOR('',#9411,0.165);
#2622=VECTOR('',#9418,0.165);
#2623=VECTOR('',#9425,2.35);
#2624=VECTOR('',#9436,2.15);
#2625=VECTOR('',#9441,0.25);
#2626=VECTOR('',#9450,0.25);
#2627=VECTOR('',#9457,1.);
#2628=VECTOR('',#9458,1.);
#2629=VECTOR('',#9459,1.);
#2630=VECTOR('',#9460,1.);
#2631=VECTOR('',#9463,1.);
#2632=VECTOR('',#9464,1.);
#2633=VECTOR('',#9465,1.);
#2634=VECTOR('',#9468,1.);
#2635=VECTOR('',#9469,1.);
#2636=VECTOR('',#9470,1.);
#2637=VECTOR('',#9473,1.);
#2638=VECTOR('',#9474,1.);
#2639=VECTOR('',#9485,0.225);
#2640=VECTOR('',#9492,0.225);
#2641=VECTOR('',#9499,0.225);
#2642=VECTOR('',#9504,1.);
#2643=VECTOR('',#9505,1.);
#2644=VECTOR('',#9506,1.);
#2645=VECTOR('',#9507,1.);
#2646=VECTOR('',#9520,2.34);
#2647=VECTOR('',#9531,1.8);
#2648=VECTOR('',#9538,1.);
#2649=VECTOR('',#9539,1.);
#2650=VECTOR('',#9540,1.);
#2651=VECTOR('',#9541,1.);
#2652=VECTOR('',#9544,1.);
#2653=VECTOR('',#9545,1.);
#2654=VECTOR('',#9546,1.);
#2655=VECTOR('',#9553,1.);
#2656=VECTOR('',#9554,1.);
#2657=VECTOR('',#9557,1.);
#2658=VECTOR('',#9558,1.);
#2659=VECTOR('',#9561,1.);
#2660=VECTOR('',#9570,0.475);
#2661=VECTOR('',#9579,0.475);
#2662=VECTOR('',#9586,0.275);
#2663=VECTOR('',#9589,0.275);
#2664=VECTOR('',#9596,1.);
#2665=VECTOR('',#9597,1.);
#2666=VECTOR('',#9598,1.);
#2667=VECTOR('',#9599,1.);
#2668=VECTOR('',#9602,1.);
#2669=VECTOR('',#9603,1.);
#2670=VECTOR('',#9604,1.);
#2671=VECTOR('',#9607,1.);
#2672=VECTOR('',#9608,1.);
#2673=VECTOR('',#9609,1.);
#2674=VECTOR('',#9612,1.);
#2675=VECTOR('',#9613,1.);
#2676=VECTOR('',#9614,1.);
#2677=VECTOR('',#9617,1.);
#2678=VECTOR('',#9618,1.);
#2679=VECTOR('',#9619,1.);
#2680=VECTOR('',#9622,1.);
#2681=VECTOR('',#9623,1.);
#2682=VECTOR('',#9640,0.475);
#2683=VECTOR('',#9645,0.5);
#2684=VECTOR('',#9650,0.485);
#2685=VECTOR('',#9659,0.31);
#2686=VECTOR('',#9662,0.3);
#2687=VECTOR('',#9681,1.63531);
#2688=VECTOR('',#9688,1.);
#2689=VECTOR('',#9693,1.05);
#2690=VECTOR('',#9702,1.63531);
#2691=VECTOR('',#9709,1.05);
#2692=VECTOR('',#9728,1.71469);
#2693=VECTOR('',#9739,2.3);
#2694=VECTOR('',#9744,2.35);
#2695=VECTOR('',#9749,2.3);
#2696=VECTOR('',#9754,1.71469);
#2697=VECTOR('',#9805,1.706752);
#2698=VECTOR('',#9882,1.643248);
#2699=VECTOR('',#9911,1.70469);
#2700=VECTOR('',#9918,1.65031);
#2701=VECTOR('',#9929,1.70469);
#2702=VECTOR('',#9936,1.65031);
#2703=VECTOR('',#9955,0.165);
#2704=VECTOR('',#9964,0.165);
#2705=VECTOR('',#9973,0.165);
#2706=VECTOR('',#9982,0.21);
#2707=VECTOR('',#9991,0.21);
#2708=VECTOR('',#10000,0.475);
#2709=VECTOR('',#10011,0.210000000000001);
#2710=VECTOR('',#10016,0.475);
#2711=VECTOR('',#10027,0.210000000000001);
#2712=VECTOR('',#10032,1.11);
#2713=VECTOR('',#10037,1.);
#2714=VECTOR('',#10038,1.);
#2715=VECTOR('',#10039,1.);
#2716=VECTOR('',#10040,1.);
#2717=VECTOR('',#10043,1.);
#2718=VECTOR('',#10044,1.);
#2719=VECTOR('',#10045,1.);
#2720=VECTOR('',#10048,1.);
#2721=VECTOR('',#10049,1.);
#2722=VECTOR('',#10050,1.);
#2723=VECTOR('',#10053,1.);
#2724=VECTOR('',#10054,1.);
#2725=VECTOR('',#10055,1.);
#2726=VECTOR('',#10056,1.);
#2727=VECTOR('',#10057,1.);
#2728=VECTOR('',#10060,1.);
#2729=VECTOR('',#10061,1.);
#2730=VECTOR('',#10064,1.);
#2731=VECTOR('',#10065,1.);
#2732=VECTOR('',#10068,1.);
#2733=VECTOR('',#10069,1.);
#2734=VECTOR('',#10070,1.);
#2735=VECTOR('',#10073,1.);
#2736=VECTOR('',#10074,1.);
#2737=VECTOR('',#10083,1.);
#2738=VECTOR('',#10084,1.);
#2739=VECTOR('',#10085,1.);
#2740=VECTOR('',#10086,1.);
#2741=VECTOR('',#10089,1.);
#2742=VECTOR('',#10090,1.);
#2743=VECTOR('',#10091,1.);
#2744=VECTOR('',#10094,1.);
#2745=VECTOR('',#10095,1.);
#2746=VECTOR('',#10096,1.);
#2747=VECTOR('',#10099,1.);
#2748=VECTOR('',#10100,1.);
#2749=VECTOR('',#10109,1.);
#2750=VECTOR('',#10110,1.);
#2751=VECTOR('',#10111,1.);
#2752=VECTOR('',#10112,1.);
#2753=VECTOR('',#10115,1.);
#2754=VECTOR('',#10116,1.);
#2755=VECTOR('',#10117,1.);
#2756=VECTOR('',#10124,1.);
#2757=VECTOR('',#10125,1.);
#2758=VECTOR('',#10128,1.);
#2759=VECTOR('',#10129,1.);
#2760=VECTOR('',#10132,1.);
#2761=VECTOR('',#10139,0.475);
#2762=VECTOR('',#10148,0.475);
#2763=VECTOR('',#10157,0.275);
#2764=VECTOR('',#10160,0.275);
#2765=VECTOR('',#10167,0.45);
#2766=VECTOR('',#10172,0.45);
#2767=VECTOR('',#10175,0.45);
#2768=VECTOR('',#10178,0.45);
#2769=VECTOR('',#10181,0.45);
#2770=VECTOR('',#10184,0.45);
#2771=VECTOR('',#10187,0.45);
#2772=VECTOR('',#10190,0.45);
#2773=VECTOR('',#10193,0.45);
#2774=VECTOR('',#10198,0.625);
#2775=VECTOR('',#10203,0.625);
#2776=VECTOR('',#10206,0.625);
#2777=VECTOR('',#10209,0.625);
#2778=VECTOR('',#10212,0.625);
#2779=VECTOR('',#10215,0.625);
#2780=VECTOR('',#10218,0.625);
#2781=VECTOR('',#10221,0.625);
#2782=VECTOR('',#10224,0.625);
#2783=VECTOR('',#10231,1.);
#2784=VECTOR('',#10246,0.225);
#2785=VECTOR('',#10251,0.225);
#2786=VECTOR('',#10256,0.225);
#2787=VECTOR('',#10259,1.);
#2788=VECTOR('',#10260,1.);
#2789=VECTOR('',#10261,1.);
#2790=VECTOR('',#10274,1.1);
#2791=VECTOR('',#10289,0.4);
#2792=VECTOR('',#10294,0.425);
#2793=VECTOR('',#10299,0.41);
#2794=VECTOR('',#10308,0.26);
#2795=VECTOR('',#10313,0.25);
#2796=VECTOR('',#10318,0.225);
#2797=VECTOR('',#10323,1.);
#2798=VECTOR('',#10324,1.);
#2799=VECTOR('',#10325,1.);
#2800=VECTOR('',#10326,1.);
#2801=VECTOR('',#10329,1.);
#2802=VECTOR('',#10330,1.);
#2803=VECTOR('',#10331,1.);
#2804=VECTOR('',#10334,1.);
#2805=VECTOR('',#10335,1.);
#2806=VECTOR('',#10336,1.);
#2807=VECTOR('',#10339,1.);
#2808=VECTOR('',#10340,1.);
#2809=VECTOR('',#10341,1.);
#2810=VECTOR('',#10344,1.);
#2811=VECTOR('',#10345,1.);
#2812=VECTOR('',#10346,1.);
#2813=VECTOR('',#10349,1.);
#2814=VECTOR('',#10350,1.);
#2815=VECTOR('',#10365,0.325);
#2816=VECTOR('',#10370,0.35);
#2817=VECTOR('',#10375,0.335);
#2818=VECTOR('',#10384,0.21);
#2819=VECTOR('',#10389,0.2);
#2820=VECTOR('',#10394,0.18);
#2821=VECTOR('',#10399,1.);
#2822=VECTOR('',#10400,1.);
#2823=VECTOR('',#10401,1.);
#2824=VECTOR('',#10402,1.);
#2825=VECTOR('',#10405,1.);
#2826=VECTOR('',#10406,1.);
#2827=VECTOR('',#10407,1.);
#2828=VECTOR('',#10410,1.);
#2829=VECTOR('',#10411,1.);
#2830=VECTOR('',#10412,1.);
#2831=VECTOR('',#10415,1.);
#2832=VECTOR('',#10416,1.);
#2833=VECTOR('',#10417,1.);
#2834=VECTOR('',#10420,1.);
#2835=VECTOR('',#10421,1.);
#2836=VECTOR('',#10422,1.);
#2837=VECTOR('',#10425,1.);
#2838=VECTOR('',#10426,1.);
#2839=VECTOR('',#10459,0.6);
#2840=VECTOR('',#10464,0.6);
#2841=VECTOR('',#10467,0.6);
#2842=VECTOR('',#10470,0.6);
#2843=VECTOR('',#10473,0.6);
#2844=VECTOR('',#10476,0.6);
#2845=VECTOR('',#10479,0.6);
#2846=VECTOR('',#10482,0.6);
#2847=VECTOR('',#10485,0.6);
#2848=VECTOR('',#10488,0.6);
#2849=VECTOR('',#10491,0.6);
#2850=VECTOR('',#10494,0.6);
#2851=VECTOR('',#10497,0.6);
#2852=VECTOR('',#10500,0.6);
#2853=VECTOR('',#10503,0.6);
#2854=VECTOR('',#10506,0.6);
#2855=VECTOR('',#10509,0.6);
#2856=VECTOR('',#10512,0.6);
#2857=VECTOR('',#10515,0.6);
#2858=VECTOR('',#10518,0.6);
#2859=VECTOR('',#10521,0.6);
#2860=VECTOR('',#10524,0.6);
#2861=VECTOR('',#10527,0.6);
#2862=VECTOR('',#10530,0.6);
#2863=VECTOR('',#10533,0.6);
#2864=VECTOR('',#10536,0.6);
#2865=VECTOR('',#10539,0.6);
#2866=VECTOR('',#10542,0.6);
#2867=VECTOR('',#10545,0.6);
#2868=VECTOR('',#10548,0.6);
#2869=VECTOR('',#10551,0.6);
#2870=VECTOR('',#10554,0.6);
#2871=VECTOR('',#10557,0.6);
#2872=VECTOR('',#10560,0.6);
#2873=VECTOR('',#10563,0.6);
#2874=VECTOR('',#10566,0.6);
#2875=VECTOR('',#10569,0.6);
#2876=VECTOR('',#10572,0.6);
#2877=VECTOR('',#10575,0.6);
#2878=VECTOR('',#10578,0.6);
#2879=VECTOR('',#10581,0.6);
#2880=VECTOR('',#10584,0.6);
#2881=VECTOR('',#10587,0.6);
#2882=VECTOR('',#10590,0.6);
#2883=VECTOR('',#10593,0.6);
#2884=VECTOR('',#10596,0.6);
#2885=VECTOR('',#10599,0.6);
#2886=VECTOR('',#10602,0.6);
#2887=VECTOR('',#10605,0.6);
#2888=VECTOR('',#10608,0.6);
#2889=VECTOR('',#10611,0.6);
#2890=VECTOR('',#10614,0.6);
#2891=VECTOR('',#10617,0.6);
#2892=VECTOR('',#10620,0.6);
#2893=VECTOR('',#10623,0.6);
#2894=VECTOR('',#10626,0.6);
#2895=VECTOR('',#10629,0.6);
#2896=VECTOR('',#10632,0.6);
#2897=VECTOR('',#10635,0.6);
#2898=VECTOR('',#10638,0.6);
#2899=VECTOR('',#10641,0.6);
#2900=VECTOR('',#10644,0.6);
#2901=VECTOR('',#10647,0.6);
#2902=VECTOR('',#10650,0.415875);
#2903=VECTOR('',#10655,0.415875);
#2904=VECTOR('',#10660,0.415875);
#2905=VECTOR('',#10663,0.415875);
#2906=VECTOR('',#10666,0.415875);
#2907=VECTOR('',#10669,0.415875);
#2908=VECTOR('',#10672,0.415875);
#2909=VECTOR('',#10675,0.415875);
#2910=VECTOR('',#10678,0.415875);
#2911=VECTOR('',#10681,0.415875);
#2912=VECTOR('',#10684,0.415875);
#2913=VECTOR('',#10687,0.415875);
#2914=VECTOR('',#10690,0.415875);
#2915=VECTOR('',#10693,0.415875);
#2916=VECTOR('',#10696,0.415875);
#2917=VECTOR('',#10699,0.415875);
#2918=VECTOR('',#10702,0.415875);
#2919=VECTOR('',#10705,0.415875);
#2920=VECTOR('',#10708,0.415875);
#2921=VECTOR('',#10711,0.415875);
#2922=VECTOR('',#10714,0.415875);
#2923=VECTOR('',#10717,0.415875);
#2924=VECTOR('',#10720,0.415875);
#2925=VECTOR('',#10723,0.415875);
#2926=VECTOR('',#10726,0.415875);
#2927=VECTOR('',#10729,0.415875);
#2928=VECTOR('',#10732,0.415875);
#2929=VECTOR('',#10735,0.415875);
#2930=VECTOR('',#10738,0.415875);
#2931=VECTOR('',#10741,0.415875);
#2932=VECTOR('',#10744,0.415875);
#2933=VECTOR('',#10747,0.415875);
#2934=VECTOR('',#10750,0.415875);
#2935=VECTOR('',#10753,0.415875);
#2936=VECTOR('',#10756,0.415875);
#2937=VECTOR('',#10759,0.415875);
#2938=VECTOR('',#10762,0.415875);
#2939=VECTOR('',#10765,0.415875);
#2940=VECTOR('',#10768,0.415875);
#2941=VECTOR('',#10771,0.415875);
#2942=VECTOR('',#10774,0.415875);
#2943=VECTOR('',#10777,0.415875);
#2944=VECTOR('',#10780,0.415875);
#2945=VECTOR('',#10783,0.415875);
#2946=VECTOR('',#10786,0.415875);
#2947=VECTOR('',#10789,0.415875);
#2948=VECTOR('',#10792,0.415875);
#2949=VECTOR('',#10795,0.415875);
#2950=VECTOR('',#10798,0.415875);
#2951=VECTOR('',#10801,0.415875);
#2952=VECTOR('',#10804,0.415875);
#2953=VECTOR('',#10807,0.415875);
#2954=VECTOR('',#10810,0.415875);
#2955=VECTOR('',#10813,0.415875);
#2956=VECTOR('',#10816,0.415875);
#2957=VECTOR('',#10819,0.415875);
#2958=VECTOR('',#10822,0.415875);
#2959=VECTOR('',#10825,0.415875);
#2960=VECTOR('',#10828,0.415875);
#2961=VECTOR('',#10831,0.415875);
#2962=VECTOR('',#10834,0.415875);
#2963=VECTOR('',#10837,0.415875);
#2964=VECTOR('',#10840,0.415875);
#2965=VECTOR('',#10847,1.);
#2966=VECTOR('',#10848,1.);
#2967=VECTOR('',#10849,1.);
#2968=VECTOR('',#10850,1.);
#2969=VECTOR('',#10855,1.);
#2970=VECTOR('',#10856,1.);
#2971=VECTOR('',#10859,1.);
#2972=VECTOR('',#10860,1.);
#2973=VECTOR('',#10863,1.);
#2974=VECTOR('',#10864,1.);
#2975=VECTOR('',#10873,1.);
#2976=VECTOR('',#10888,1.35);
#2977=VECTOR('',#10901,1.01);
#2978=VECTOR('',#10908,1.35);
#2979=VECTOR('',#10919,1.);
#2980=VECTOR('',#10926,0.210000000000001);
#2981=VECTOR('',#10929,1.);
#2982=VECTOR('',#10934,1.005);
#2983=VECTOR('',#10941,1.5);
#2984=VECTOR('',#10954,0.25);
#2985=VECTOR('',#10959,1.);
#2986=VECTOR('',#10966,0.210000000000001);
#2987=VECTOR('',#10969,1.);
#2988=VECTOR('',#10972,1.);
#2989=VECTOR('',#10973,1.);
#2990=VECTOR('',#10974,1.);
#2991=VECTOR('',#10975,1.);
#2992=VECTOR('',#10976,1.);
#2993=VECTOR('',#10977,1.);
#2994=VECTOR('',#10980,1.);
#2995=VECTOR('',#10981,1.);
#2996=VECTOR('',#10982,1.);
#2997=VECTOR('',#10985,1.);
#2998=VECTOR('',#10986,1.);
#2999=VECTOR('',#10987,1.);
#3000=VECTOR('',#10988,1.);
#3001=VECTOR('',#10989,1.);
#3002=VECTOR('',#11004,3.5);
#3003=VECTOR('',#11021,0.33);
#3004=VECTOR('',#11028,0.4);
#3005=VECTOR('',#11041,0.405);
#3006=VECTOR('',#11048,0.9);
#3007=VECTOR('',#11059,1.);
#3008=VECTOR('',#11060,1.);
#3009=VECTOR('',#11061,1.);
#3010=VECTOR('',#11062,1.);
#3011=VECTOR('',#11063,1.);
#3012=VECTOR('',#11064,1.);
#3013=VECTOR('',#11065,1.);
#3014=VECTOR('',#11066,1.);
#3015=VECTOR('',#11069,1.);
#3016=VECTOR('',#11070,1.);
#3017=VECTOR('',#11071,1.);
#3018=VECTOR('',#11074,1.);
#3019=VECTOR('',#11075,1.);
#3020=VECTOR('',#11078,1.);
#3021=VECTOR('',#11079,1.);
#3022=VECTOR('',#11082,1.);
#3023=VECTOR('',#11083,1.);
#3024=VECTOR('',#11086,1.);
#3025=VECTOR('',#11087,1.);
#3026=VECTOR('',#11088,1.);
#3027=VECTOR('',#11089,1.);
#3028=VECTOR('',#11092,1.);
#3029=VECTOR('',#11095,1.);
#3030=VECTOR('',#11098,1.);
#3031=VECTOR('',#11105,1.);
#3032=VECTOR('',#11106,1.);
#3033=VECTOR('',#11107,1.);
#3034=VECTOR('',#11108,1.);
#3035=VECTOR('',#11111,1.);
#3036=VECTOR('',#11112,1.);
#3037=VECTOR('',#11113,1.);
#3038=VECTOR('',#11116,1.);
#3039=VECTOR('',#11117,1.);
#3040=VECTOR('',#11118,1.);
#3041=VECTOR('',#11121,1.);
#3042=VECTOR('',#11122,1.);
#3043=VECTOR('',#11123,1.);
#3044=VECTOR('',#11126,1.);
#3045=VECTOR('',#11127,1.);
#3046=VECTOR('',#11128,1.);
#3047=VECTOR('',#11131,1.);
#3048=VECTOR('',#11132,1.);
#3049=VECTOR('',#11143,0.235);
#3050=VECTOR('',#11148,0.25);
#3051=VECTOR('',#11153,0.2125);
#3052=VECTOR('',#11162,0.32);
#3053=VECTOR('',#11169,0.6);
#3054=VECTOR('',#11186,0.475);
#3055=VECTOR('',#11191,0.5);
#3056=VECTOR('',#11196,0.485);
#3057=VECTOR('',#11205,0.31);
#3058=VECTOR('',#11210,0.3);
#3059=VECTOR('',#11215,0.27);
#3060=VECTOR('',#11220,1.);
#3061=VECTOR('',#11221,1.);
#3062=VECTOR('',#11222,1.);
#3063=VECTOR('',#11223,1.);
#3064=VECTOR('',#11226,1.);
#3065=VECTOR('',#11227,1.);
#3066=VECTOR('',#11228,1.);
#3067=VECTOR('',#11231,1.);
#3068=VECTOR('',#11232,1.);
#3069=VECTOR('',#11233,1.);
#3070=VECTOR('',#11236,1.);
#3071=VECTOR('',#11237,1.);
#3072=VECTOR('',#11238,1.);
#3073=VECTOR('',#11241,1.);
#3074=VECTOR('',#11242,1.);
#3075=VECTOR('',#11243,1.);
#3076=VECTOR('',#11246,1.);
#3077=VECTOR('',#11247,1.);
#3078=CIRCLE('',#8405,0.33);
#3079=CIRCLE('',#8406,0.33);
#3080=CIRCLE('',#8408,0.33);
#3081=CIRCLE('',#8409,0.33);
#3082=CIRCLE('',#8411,0.329999999999998);
#3083=CIRCLE('',#8412,0.329999999999998);
#3084=CIRCLE('',#8414,0.33);
#3085=CIRCLE('',#8415,0.33);
#3086=CIRCLE('',#8417,0.329999999999998);
#3087=CIRCLE('',#8418,0.329999999999998);
#3088=CIRCLE('',#8420,0.33);
#3089=CIRCLE('',#8421,0.33);
#3090=CIRCLE('',#8423,0.329999999999998);
#3091=CIRCLE('',#8424,0.329999999999998);
#3092=CIRCLE('',#8433,0.25);
#3093=CIRCLE('',#8434,0.25);
#3094=CIRCLE('',#8437,0.25);
#3095=CIRCLE('',#8438,0.25);
#3096=CIRCLE('',#8441,0.25);
#3097=CIRCLE('',#8442,0.25);
#3098=CIRCLE('',#8452,0.21);
#3099=CIRCLE('',#8453,0.21);
#3100=CIRCLE('',#8456,0.21);
#3101=CIRCLE('',#8457,0.21);
#3102=CIRCLE('',#8460,0.25);
#3103=CIRCLE('',#8461,0.25);
#3104=CIRCLE('',#8464,0.25);
#3105=CIRCLE('',#8465,0.25);
#3106=CIRCLE('',#8475,0.165);
#3107=CIRCLE('',#8476,0.165);
#3108=CIRCLE('',#8478,0.165);
#3109=CIRCLE('',#8479,0.165);
#3110=CIRCLE('',#8481,0.165);
#3111=CIRCLE('',#8482,0.165);
#3112=CIRCLE('',#8484,2.35);
#3113=CIRCLE('',#8485,2.35);
#3114=CIRCLE('',#8487,2.15);
#3115=CIRCLE('',#8489,2.15);
#3116=CIRCLE('',#8491,0.25);
#3117=CIRCLE('',#8492,0.25);
#3118=CIRCLE('',#8495,0.25);
#3119=CIRCLE('',#8496,0.25);
#3120=CIRCLE('',#8506,0.225);
#3121=CIRCLE('',#8507,0.225);
#3122=CIRCLE('',#8509,0.225);
#3123=CIRCLE('',#8510,0.225);
#3124=CIRCLE('',#8512,0.225);
#3125=CIRCLE('',#8513,0.225);
#3126=CIRCLE('',#8516,3.);
#3127=CIRCLE('',#8517,2.34);
#3128=CIRCLE('',#8519,3.);
#3129=CIRCLE('',#8521,2.34);
#3130=CIRCLE('',#8523,1.8);
#3131=CIRCLE('',#8525,1.8);
#3132=CIRCLE('',#8530,0.275);
#3133=CIRCLE('',#8531,0.275);
#3134=CIRCLE('',#8535,0.475);
#3135=CIRCLE('',#8536,0.475);
#3136=CIRCLE('',#8538,0.475);
#3137=CIRCLE('',#8540,0.275);
#3138=CIRCLE('',#8542,0.475);
#3139=CIRCLE('',#8544,0.275);
#3140=CIRCLE('',#8558,0.2942);
#3141=CIRCLE('',#8560,0.45);
#3142=CIRCLE('',#8562,0.5);
#3143=CIRCLE('',#8564,0.5);
#3144=CIRCLE('',#8566,0.47);
#3145=CIRCLE('',#8568,0.32);
#3146=CIRCLE('',#8570,0.2942);
#3147=CIRCLE('',#8575,1.63531);
#3148=CIRCLE('',#8576,1.63531);
#3149=CIRCLE('',#8577,0.412776);
#3150=CIRCLE('',#8578,1.63531);
#3151=CIRCLE('',#8579,1.63531);
#3152=CIRCLE('',#8581,1.63531);
#3153=CIRCLE('',#8583,1.);
#3154=CIRCLE('',#8584,1.);
#3155=CIRCLE('',#8586,1.1);
#3156=CIRCLE('',#8589,1.63531);
#3157=CIRCLE('',#8591,1.1);
#3158=CIRCLE('',#8595,1.71469);
#3159=CIRCLE('',#8596,1.71469);
#3160=CIRCLE('',#8597,0.412776);
#3161=CIRCLE('',#8598,1.71469);
#3162=CIRCLE('',#8599,1.71469);
#3163=CIRCLE('',#8601,1.71469);
#3164=CIRCLE('',#8603,2.25);
#3165=CIRCLE('',#8604,1.71469);
#3166=CIRCLE('',#8606,2.35);
#3167=CIRCLE('',#8608,2.35);
#3168=CIRCLE('',#8610,2.25);
#3169=CIRCLE('',#8615,0.3969);
#3170=CIRCLE('',#8617,0.3969);
#3171=CIRCLE('',#8619,0.3969);
#3172=CIRCLE('',#8621,0.3969);
#3173=CIRCLE('',#8623,0.3969);
#3174=CIRCLE('',#8625,0.3969);
#3175=CIRCLE('',#8627,0.3969);
#3176=CIRCLE('',#8629,0.3969);
#3177=CIRCLE('',#8632,0.405071403305639);
#3178=CIRCLE('',#8633,0.405071403305639);
#3179=CIRCLE('',#8635,1.706752);
#3180=CIRCLE('',#8636,1.706752);
#3181=CIRCLE('',#8637,1.706752);
#3182=CIRCLE('',#8638,1.706752);
#3183=CIRCLE('',#8639,1.706752);
#3184=CIRCLE('',#8640,1.706752);
#3185=CIRCLE('',#8641,1.706752);
#3186=CIRCLE('',#8642,1.706752);
#3187=CIRCLE('',#8643,1.706752);
#3188=CIRCLE('',#8645,1.643248);
#3189=CIRCLE('',#8646,0.405071403305639);
#3190=CIRCLE('',#8648,0.405071403305639);
#3191=CIRCLE('',#8650,1.643248);
#3192=CIRCLE('',#8651,0.405071403305639);
#3193=CIRCLE('',#8653,0.405071403305639);
#3194=CIRCLE('',#8655,1.643248);
#3195=CIRCLE('',#8656,0.405071403305639);
#3196=CIRCLE('',#8658,0.405071403305639);
#3197=CIRCLE('',#8660,1.643248);
#3198=CIRCLE('',#8661,0.405071403305639);
#3199=CIRCLE('',#8663,0.405071403305639);
#3200=CIRCLE('',#8665,1.643248);
#3201=CIRCLE('',#8666,0.405071403305639);
#3202=CIRCLE('',#8668,0.405071403305639);
#3203=CIRCLE('',#8670,1.643248);
#3204=CIRCLE('',#8671,0.405071403305639);
#3205=CIRCLE('',#8673,0.405071403305639);
#3206=CIRCLE('',#8675,1.643248);
#3207=CIRCLE('',#8676,1.643248);
#3208=CIRCLE('',#8677,1.643248);
#3209=CIRCLE('',#8679,0.405071403305639);
#3210=CIRCLE('',#8681,0.405071403305639);
#3211=CIRCLE('',#8686,1.70469);
#3212=CIRCLE('',#8687,1.65031);
#3213=CIRCLE('',#8689,1.70469);
#3214=CIRCLE('',#8691,1.65031);
#3215=CIRCLE('',#8694,1.70469);
#3216=CIRCLE('',#8695,1.65031);
#3217=CIRCLE('',#8697,1.70469);
#3218=CIRCLE('',#8699,1.65031);
#3219=CIRCLE('',#8709,0.165);
#3220=CIRCLE('',#8710,0.165);
#3221=CIRCLE('',#8713,0.165);
#3222=CIRCLE('',#8714,0.165);
#3223=CIRCLE('',#8717,0.165);
#3224=CIRCLE('',#8718,0.165);
#3225=CIRCLE('',#8721,0.21);
#3226=CIRCLE('',#8722,0.21);
#3227=CIRCLE('',#8725,0.21);
#3228=CIRCLE('',#8726,0.21);
#3229=CIRCLE('',#8729,0.475);
#3230=CIRCLE('',#8730,0.475);
#3231=CIRCLE('',#8732,0.210000000000001);
#3232=CIRCLE('',#8734,0.210000000000001);
#3233=CIRCLE('',#8736,0.475);
#3234=CIRCLE('',#8737,0.475);
#3235=CIRCLE('',#8739,0.210000000000001);
#3236=CIRCLE('',#8741,0.210000000000001);
#3237=CIRCLE('',#8743,1.11);
#3238=CIRCLE('',#8744,1.11);
#3239=CIRCLE('',#8765,0.475);
#3240=CIRCLE('',#8766,0.475);
#3241=CIRCLE('',#8770,0.275);
#3242=CIRCLE('',#8771,0.275);
#3243=CIRCLE('',#8773,0.475);
#3244=CIRCLE('',#8775,0.275);
#3245=CIRCLE('',#8777,0.475);
#3246=CIRCLE('',#8779,0.275);
#3247=CIRCLE('',#8785,0.457875);
#3248=CIRCLE('',#8794,0.457875);
#3249=CIRCLE('',#8796,0.625);
#3250=CIRCLE('',#8805,0.625);
#3251=CIRCLE('',#8808,1.9);
#3252=CIRCLE('',#8809,0.457875);
#3253=CIRCLE('',#8810,0.225);
#3254=CIRCLE('',#8811,0.225);
#3255=CIRCLE('',#8812,0.225);
#3256=CIRCLE('',#8814,0.225);
#3257=CIRCLE('',#8816,0.225);
#3258=CIRCLE('',#8818,0.225);
#3259=CIRCLE('',#8821,1.9);
#3260=CIRCLE('',#8822,1.1);
#3261=CIRCLE('',#8826,1.1);
#3262=CIRCLE('',#8830,0.375);
#3263=CIRCLE('',#8832,0.425);
#3264=CIRCLE('',#8834,0.425);
#3265=CIRCLE('',#8836,0.395);
#3266=CIRCLE('',#8838,0.27);
#3267=CIRCLE('',#8840,0.24505);
#3268=CIRCLE('',#8842,0.24505);
#3269=CIRCLE('',#8844,0.2);
#3270=CIRCLE('',#8856,0.3);
#3271=CIRCLE('',#8858,0.35);
#3272=CIRCLE('',#8860,0.35);
#3273=CIRCLE('',#8862,0.32);
#3274=CIRCLE('',#8864,0.22);
#3275=CIRCLE('',#8866,0.1954);
#3276=CIRCLE('',#8868,0.1954);
#3277=CIRCLE('',#8870,0.16);
#3278=CIRCLE('',#8894,0.5941);
#3279=CIRCLE('',#8958,0.415875);
#3280=CIRCLE('',#8960,0.415875);
#3281=CIRCLE('',#9023,0.415875);
#3282=CIRCLE('',#9026,1.);
#3283=CIRCLE('',#9030,1.);
#3284=CIRCLE('',#9032,1.);
#3285=CIRCLE('',#9033,1.);
#3286=CIRCLE('',#9036,1.35);
#3287=CIRCLE('',#9037,0.5941);
#3288=CIRCLE('',#9039,1.35);
#3289=CIRCLE('',#9045,1.01);
#3290=CIRCLE('',#9046,1.01);
#3291=CIRCLE('',#9048,1.35);
#3292=CIRCLE('',#9049,1.35);
#3293=CIRCLE('',#9054,0.210000000000001);
#3294=CIRCLE('',#9056,0.210000000000001);
#3295=CIRCLE('',#9059,1.005);
#3296=CIRCLE('',#9060,1.005);
#3297=CIRCLE('',#9062,1.5);
#3298=CIRCLE('',#9063,1.5);
#3299=CIRCLE('',#9068,0.25);
#3300=CIRCLE('',#9069,0.25);
#3301=CIRCLE('',#9071,0.210000000000001);
#3302=CIRCLE('',#9073,0.210000000000001);
#3303=CIRCLE('',#9079,3.5);
#3304=CIRCLE('',#9080,1.);
#3305=CIRCLE('',#9082,3.5);
#3306=CIRCLE('',#9083,1.5);
#3307=CIRCLE('',#9086,1.);
#3308=CIRCLE('',#9088,1.5);
#3309=CIRCLE('',#9092,0.33);
#3310=CIRCLE('',#9093,0.33);
#3311=CIRCLE('',#9095,0.4);
#3312=CIRCLE('',#9096,0.4);
#3313=CIRCLE('',#9101,0.405);
#3314=CIRCLE('',#9102,0.405);
#3315=CIRCLE('',#9104,0.9);
#3316=CIRCLE('',#9105,0.9);
#3317=CIRCLE('',#9128,0.22);
#3318=CIRCLE('',#9130,0.24505);
#3319=CIRCLE('',#9132,0.24505);
#3320=CIRCLE('',#9134,0.175);
#3321=CIRCLE('',#9138,0.32);
#3322=CIRCLE('',#9139,0.32);
#3323=CIRCLE('',#9141,0.6);
#3324=CIRCLE('',#9142,0.6);
#3325=CIRCLE('',#9147,0.45);
#3326=CIRCLE('',#9149,0.5);
#3327=CIRCLE('',#9151,0.5);
#3328=CIRCLE('',#9153,0.47);
#3329=CIRCLE('',#9155,0.32);
#3330=CIRCLE('',#9157,0.2942);
#3331=CIRCLE('',#9159,0.2942);
#3332=CIRCLE('',#9161,0.24);
#3333=VERTEX_POINT('',#11322);
#3334=VERTEX_POINT('',#11324);
#3335=VERTEX_POINT('',#11328);
#3336=VERTEX_POINT('',#11330);
#3337=VERTEX_POINT('',#11334);
#3338=VERTEX_POINT('',#11336);
#3339=VERTEX_POINT('',#11340);
#3340=VERTEX_POINT('',#11342);
#3341=VERTEX_POINT('',#11346);
#3342=VERTEX_POINT('',#11348);
#3343=VERTEX_POINT('',#11352);
#3344=VERTEX_POINT('',#11354);
#3345=VERTEX_POINT('',#11358);
#3346=VERTEX_POINT('',#11360);
#3347=VERTEX_POINT('',#11364);
#3348=VERTEX_POINT('',#11365);
#3349=VERTEX_POINT('',#11367);
#3350=VERTEX_POINT('',#11369);
#3351=VERTEX_POINT('',#11373);
#3352=VERTEX_POINT('',#11375);
#3353=VERTEX_POINT('',#11379);
#3354=VERTEX_POINT('',#11381);
#3355=VERTEX_POINT('',#11391);
#3356=VERTEX_POINT('',#11393);
#3357=VERTEX_POINT('',#11398);
#3358=VERTEX_POINT('',#11400);
#3359=VERTEX_POINT('',#11405);
#3360=VERTEX_POINT('',#11407);
#3361=VERTEX_POINT('',#11412);
#3362=VERTEX_POINT('',#11413);
#3363=VERTEX_POINT('',#11415);
#3364=VERTEX_POINT('',#11417);
#3365=VERTEX_POINT('',#11421);
#3366=VERTEX_POINT('',#11423);
#3367=VERTEX_POINT('',#11427);
#3368=VERTEX_POINT('',#11429);
#3369=VERTEX_POINT('',#11439);
#3370=VERTEX_POINT('',#11441);
#3371=VERTEX_POINT('',#11446);
#3372=VERTEX_POINT('',#11448);
#3373=VERTEX_POINT('',#11453);
#3374=VERTEX_POINT('',#11455);
#3375=VERTEX_POINT('',#11460);
#3376=VERTEX_POINT('',#11462);
#3377=VERTEX_POINT('',#11467);
#3378=VERTEX_POINT('',#11468);
#3379=VERTEX_POINT('',#11470);
#3380=VERTEX_POINT('',#11472);
#3381=VERTEX_POINT('',#11476);
#3382=VERTEX_POINT('',#11478);
#3383=VERTEX_POINT('',#11482);
#3384=VERTEX_POINT('',#11484);
#3385=VERTEX_POINT('',#11494);
#3386=VERTEX_POINT('',#11496);
#3387=VERTEX_POINT('',#11500);
#3388=VERTEX_POINT('',#11502);
#3389=VERTEX_POINT('',#11506);
#3390=VERTEX_POINT('',#11508);
#3391=VERTEX_POINT('',#11512);
#3392=VERTEX_POINT('',#11514);
#3393=VERTEX_POINT('',#11518);
#3394=VERTEX_POINT('',#11521);
#3395=VERTEX_POINT('',#11525);
#3396=VERTEX_POINT('',#11527);
#3397=VERTEX_POINT('',#11532);
#3398=VERTEX_POINT('',#11534);
#3399=VERTEX_POINT('',#11539);
#3400=VERTEX_POINT('',#11540);
#3401=VERTEX_POINT('',#11542);
#3402=VERTEX_POINT('',#11544);
#3403=VERTEX_POINT('',#11548);
#3404=VERTEX_POINT('',#11550);
#3405=VERTEX_POINT('',#11554);
#3406=VERTEX_POINT('',#11556);
#3407=VERTEX_POINT('',#11566);
#3408=VERTEX_POINT('',#11568);
#3409=VERTEX_POINT('',#11572);
#3410=VERTEX_POINT('',#11574);
#3411=VERTEX_POINT('',#11578);
#3412=VERTEX_POINT('',#11580);
#3413=VERTEX_POINT('',#11584);
#3414=VERTEX_POINT('',#11585);
#3415=VERTEX_POINT('',#11587);
#3416=VERTEX_POINT('',#11589);
#3417=VERTEX_POINT('',#11594);
#3418=VERTEX_POINT('',#11599);
#3419=VERTEX_POINT('',#11603);
#3420=VERTEX_POINT('',#11606);
#3421=VERTEX_POINT('',#11612);
#3422=VERTEX_POINT('',#11613);
#3423=VERTEX_POINT('',#11615);
#3424=VERTEX_POINT('',#11617);
#3425=VERTEX_POINT('',#11621);
#3426=VERTEX_POINT('',#11623);
#3427=VERTEX_POINT('',#11626);
#3428=VERTEX_POINT('',#11628);
#3429=VERTEX_POINT('',#11631);
#3430=VERTEX_POINT('',#11635);
#3431=VERTEX_POINT('',#11640);
#3432=VERTEX_POINT('',#11642);
#3433=VERTEX_POINT('',#11645);
#3434=VERTEX_POINT('',#11649);
#3435=VERTEX_POINT('',#11652);
#3436=VERTEX_POINT('',#11656);
#3437=VERTEX_POINT('',#11665);
#3438=VERTEX_POINT('',#11666);
#3439=VERTEX_POINT('',#11668);
#3440=VERTEX_POINT('',#11670);
#3441=VERTEX_POINT('',#11674);
#3442=VERTEX_POINT('',#11676);
#3443=VERTEX_POINT('',#11680);
#3444=VERTEX_POINT('',#11682);
#3445=VERTEX_POINT('',#11686);
#3446=VERTEX_POINT('',#11688);
#3447=VERTEX_POINT('',#11692);
#3448=VERTEX_POINT('',#11694);
#3449=VERTEX_POINT('',#11703);
#3450=VERTEX_POINT('',#11706);
#3451=VERTEX_POINT('',#11709);
#3452=VERTEX_POINT('',#11713);
#3453=VERTEX_POINT('',#11717);
#3454=VERTEX_POINT('',#11721);
#3455=VERTEX_POINT('',#11724);
#3456=VERTEX_POINT('',#11732);
#3457=VERTEX_POINT('',#11733);
#3458=VERTEX_POINT('',#11736);
#3459=VERTEX_POINT('',#11738);
#3460=VERTEX_POINT('',#11742);
#3461=VERTEX_POINT('',#11746);
#3462=VERTEX_POINT('',#11748);
#3463=VERTEX_POINT('',#11752);
#3464=VERTEX_POINT('',#11757);
#3465=VERTEX_POINT('',#11761);
#3466=VERTEX_POINT('',#11767);
#3467=VERTEX_POINT('',#11768);
#3468=VERTEX_POINT('',#11771);
#3469=VERTEX_POINT('',#11773);
#3470=VERTEX_POINT('',#11777);
#3471=VERTEX_POINT('',#11781);
#3472=VERTEX_POINT('',#11783);
#3473=VERTEX_POINT('',#11786);
#3474=VERTEX_POINT('',#11790);
#3475=VERTEX_POINT('',#11794);
#3476=VERTEX_POINT('',#11802);
#3477=VERTEX_POINT('',#11803);
#3478=VERTEX_POINT('',#11806);
#3479=VERTEX_POINT('',#11807);
#3480=VERTEX_POINT('',#11810);
#3481=VERTEX_POINT('',#11811);
#3482=VERTEX_POINT('',#11814);
#3483=VERTEX_POINT('',#11815);
#3484=VERTEX_POINT('',#11818);
#3485=VERTEX_POINT('',#11819);
#3486=VERTEX_POINT('',#11822);
#3487=VERTEX_POINT('',#11823);
#3488=VERTEX_POINT('',#11826);
#3489=VERTEX_POINT('',#11827);
#3490=VERTEX_POINT('',#11830);
#3491=VERTEX_POINT('',#11831);
#3492=VERTEX_POINT('',#11835);
#3493=VERTEX_POINT('',#11836);
#3494=VERTEX_POINT('',#11859);
#3495=VERTEX_POINT('',#11861);
#3496=VERTEX_POINT('',#11886);
#3497=VERTEX_POINT('',#11888);
#3498=VERTEX_POINT('',#11911);
#3499=VERTEX_POINT('',#11913);
#3500=VERTEX_POINT('',#11936);
#3501=VERTEX_POINT('',#11938);
#3502=VERTEX_POINT('',#11951);
#3503=VERTEX_POINT('',#11954);
#3504=VERTEX_POINT('',#11967);
#3505=VERTEX_POINT('',#11969);
#3506=VERTEX_POINT('',#11992);
#3507=VERTEX_POINT('',#11994);
#3508=VERTEX_POINT('',#12017);
#3509=VERTEX_POINT('',#12019);
#3510=VERTEX_POINT('',#12042);
#3511=VERTEX_POINT('',#12044);
#3512=VERTEX_POINT('',#12069);
#3513=VERTEX_POINT('',#12073);
#3514=VERTEX_POINT('',#12098);
#3515=VERTEX_POINT('',#12102);
#3516=VERTEX_POINT('',#12127);
#3517=VERTEX_POINT('',#12131);
#3518=VERTEX_POINT('',#12132);
#3519=VERTEX_POINT('',#12159);
#3520=VERTEX_POINT('',#12163);
#3521=VERTEX_POINT('',#12188);
#3522=VERTEX_POINT('',#12192);
#3523=VERTEX_POINT('',#12217);
#3524=VERTEX_POINT('',#12221);
#3525=VERTEX_POINT('',#12246);
#3526=VERTEX_POINT('',#12249);
#3527=VERTEX_POINT('',#12251);
#3528=VERTEX_POINT('',#12283);
#3529=VERTEX_POINT('',#12285);
#3530=VERTEX_POINT('',#12288);
#3531=VERTEX_POINT('',#12292);
#3532=VERTEX_POINT('',#12297);
#3533=VERTEX_POINT('',#12299);
#3534=VERTEX_POINT('',#12302);
#3535=VERTEX_POINT('',#12306);
#3536=VERTEX_POINT('',#12318);
#3537=VERTEX_POINT('',#12320);
#3538=VERTEX_POINT('',#12325);
#3539=VERTEX_POINT('',#12327);
#3540=VERTEX_POINT('',#12332);
#3541=VERTEX_POINT('',#12334);
#3542=VERTEX_POINT('',#12339);
#3543=VERTEX_POINT('',#12341);
#3544=VERTEX_POINT('',#12346);
#3545=VERTEX_POINT('',#12348);
#3546=VERTEX_POINT('',#12353);
#3547=VERTEX_POINT('',#12355);
#3548=VERTEX_POINT('',#12359);
#3549=VERTEX_POINT('',#12362);
#3550=VERTEX_POINT('',#12366);
#3551=VERTEX_POINT('',#12368);
#3552=VERTEX_POINT('',#12372);
#3553=VERTEX_POINT('',#12375);
#3554=VERTEX_POINT('',#12379);
#3555=VERTEX_POINT('',#12381);
#3556=VERTEX_POINT('',#12385);
#3557=VERTEX_POINT('',#12386);
#3558=VERTEX_POINT('',#12388);
#3559=VERTEX_POINT('',#12390);
#3560=VERTEX_POINT('',#12394);
#3561=VERTEX_POINT('',#12396);
#3562=VERTEX_POINT('',#12400);
#3563=VERTEX_POINT('',#12402);
#3564=VERTEX_POINT('',#12406);
#3565=VERTEX_POINT('',#12408);
#3566=VERTEX_POINT('',#12410);
#3567=VERTEX_POINT('',#12412);
#3568=VERTEX_POINT('',#12416);
#3569=VERTEX_POINT('',#12420);
#3570=VERTEX_POINT('',#12424);
#3571=VERTEX_POINT('',#12426);
#3572=VERTEX_POINT('',#12436);
#3573=VERTEX_POINT('',#12437);
#3574=VERTEX_POINT('',#12439);
#3575=VERTEX_POINT('',#12441);
#3576=VERTEX_POINT('',#12445);
#3577=VERTEX_POINT('',#12447);
#3578=VERTEX_POINT('',#12451);
#3579=VERTEX_POINT('',#12453);
#3580=VERTEX_POINT('',#12463);
#3581=VERTEX_POINT('',#12464);
#3582=VERTEX_POINT('',#12466);
#3583=VERTEX_POINT('',#12468);
#3584=VERTEX_POINT('',#12472);
#3585=VERTEX_POINT('',#12474);
#3586=VERTEX_POINT('',#12477);
#3587=VERTEX_POINT('',#12479);
#3588=VERTEX_POINT('',#12482);
#3589=VERTEX_POINT('',#12486);
#3590=VERTEX_POINT('',#12491);
#3591=VERTEX_POINT('',#12493);
#3592=VERTEX_POINT('',#12496);
#3593=VERTEX_POINT('',#12500);
#3594=VERTEX_POINT('',#12503);
#3595=VERTEX_POINT('',#12507);
#3596=VERTEX_POINT('',#12516);
#3597=VERTEX_POINT('',#12517);
#3598=VERTEX_POINT('',#12519);
#3599=VERTEX_POINT('',#12545);
#3600=VERTEX_POINT('',#12588);
#3601=VERTEX_POINT('',#12589);
#3602=VERTEX_POINT('',#12675);
#3603=VERTEX_POINT('',#12676);
#3604=VERTEX_POINT('',#12765);
#3605=VERTEX_POINT('',#12766);
#3606=VERTEX_POINT('',#12852);
#3607=VERTEX_POINT('',#12853);
#3608=VERTEX_POINT('',#12942);
#3609=VERTEX_POINT('',#12943);
#3610=VERTEX_POINT('',#13029);
#3611=VERTEX_POINT('',#13030);
#3612=VERTEX_POINT('',#13116);
#3613=VERTEX_POINT('',#13117);
#3614=VERTEX_POINT('',#13206);
#3615=VERTEX_POINT('',#13207);
#3616=VERTEX_POINT('',#13209);
#3617=VERTEX_POINT('',#13222);
#3618=VERTEX_POINT('',#13223);
#3619=VERTEX_POINT('',#13225);
#3620=VERTEX_POINT('',#13233);
#3621=VERTEX_POINT('',#13248);
#3622=VERTEX_POINT('',#13249);
#3623=VERTEX_POINT('',#13285);
#3624=VERTEX_POINT('',#13286);
#3625=VERTEX_POINT('',#13322);
#3626=VERTEX_POINT('',#13323);
#3627=VERTEX_POINT('',#13360);
#3628=VERTEX_POINT('',#13361);
#3629=VERTEX_POINT('',#13397);
#3630=VERTEX_POINT('',#13398);
#3631=VERTEX_POINT('',#13434);
#3632=VERTEX_POINT('',#13435);
#3633=VERTEX_POINT('',#13472);
#3634=VERTEX_POINT('',#13473);
#3635=VERTEX_POINT('',#13510);
#3636=VERTEX_POINT('',#13511);
#3637=VERTEX_POINT('',#13513);
#3638=VERTEX_POINT('',#13519);
#3639=VERTEX_POINT('',#14583);
#3640=VERTEX_POINT('',#14675);
#3641=VERTEX_POINT('',#14676);
#3642=VERTEX_POINT('',#14680);
#3643=VERTEX_POINT('',#14682);
#3644=VERTEX_POINT('',#14684);
#3645=VERTEX_POINT('',#14687);
#3646=VERTEX_POINT('',#14691);
#3647=VERTEX_POINT('',#14695);
#3648=VERTEX_POINT('',#14699);
#3649=VERTEX_POINT('',#14700);
#3650=VERTEX_POINT('',#14706);
#3651=VERTEX_POINT('',#14711);
#3652=VERTEX_POINT('',#14717);
#3653=VERTEX_POINT('',#14720);
#3654=VERTEX_POINT('',#14724);
#3655=VERTEX_POINT('',#14728);
#3656=VERTEX_POINT('',#14732);
#3657=VERTEX_POINT('',#14735);
#3658=VERTEX_POINT('',#14739);
#3659=VERTEX_POINT('',#14743);
#3660=VERTEX_POINT('',#14748);
#3661=VERTEX_POINT('',#14749);
#3662=VERTEX_POINT('',#14751);
#3663=VERTEX_POINT('',#14753);
#3664=VERTEX_POINT('',#14757);
#3665=VERTEX_POINT('',#14759);
#3666=VERTEX_POINT('',#14763);
#3667=VERTEX_POINT('',#14765);
#3668=VERTEX_POINT('',#14769);
#3669=VERTEX_POINT('',#14771);
#3670=VERTEX_POINT('',#14775);
#3671=VERTEX_POINT('',#14777);
#3672=VERTEX_POINT('',#14787);
#3673=VERTEX_POINT('',#14790);
#3674=VERTEX_POINT('',#14794);
#3675=VERTEX_POINT('',#14798);
#3676=VERTEX_POINT('',#14802);
#3677=VERTEX_POINT('',#14805);
#3678=VERTEX_POINT('',#14809);
#3679=VERTEX_POINT('',#14813);
#3680=VERTEX_POINT('',#14818);
#3681=VERTEX_POINT('',#14819);
#3682=VERTEX_POINT('',#14821);
#3683=VERTEX_POINT('',#14823);
#3684=VERTEX_POINT('',#14827);
#3685=VERTEX_POINT('',#14829);
#3686=VERTEX_POINT('',#14833);
#3687=VERTEX_POINT('',#14835);
#3688=VERTEX_POINT('',#14839);
#3689=VERTEX_POINT('',#14841);
#3690=VERTEX_POINT('',#14845);
#3691=VERTEX_POINT('',#14847);
#3692=VERTEX_POINT('',#14869);
#3693=VERTEX_POINT('',#14870);
#3694=VERTEX_POINT('',#14872);
#3695=VERTEX_POINT('',#14892);
#3696=VERTEX_POINT('',#14899);
#3697=VERTEX_POINT('',#14900);
#3698=VERTEX_POINT('',#14986);
#3699=VERTEX_POINT('',#14987);
#3700=VERTEX_POINT('',#15076);
#3701=VERTEX_POINT('',#15077);
#3702=VERTEX_POINT('',#15163);
#3703=VERTEX_POINT('',#15164);
#3704=VERTEX_POINT('',#15250);
#3705=VERTEX_POINT('',#15251);
#3706=VERTEX_POINT('',#15337);
#3707=VERTEX_POINT('',#15338);
#3708=VERTEX_POINT('',#15424);
#3709=VERTEX_POINT('',#15425);
#3710=VERTEX_POINT('',#15511);
#3711=VERTEX_POINT('',#15512);
#3712=VERTEX_POINT('',#15583);
#3713=VERTEX_POINT('',#15584);
#3714=VERTEX_POINT('',#15634);
#3715=VERTEX_POINT('',#15635);
#3716=VERTEX_POINT('',#15682);
#3717=VERTEX_POINT('',#15683);
#3718=VERTEX_POINT('',#15730);
#3719=VERTEX_POINT('',#15731);
#3720=VERTEX_POINT('',#15781);
#3721=VERTEX_POINT('',#15782);
#3722=VERTEX_POINT('',#15832);
#3723=VERTEX_POINT('',#15833);
#3724=VERTEX_POINT('',#15880);
#3725=VERTEX_POINT('',#15881);
#3726=VERTEX_POINT('',#15931);
#3727=VERTEX_POINT('',#15932);
#3728=VERTEX_POINT('',#15982);
#3729=VERTEX_POINT('',#15983);
#3730=VERTEX_POINT('',#16030);
#3731=VERTEX_POINT('',#16031);
#3732=VERTEX_POINT('',#16078);
#3733=VERTEX_POINT('',#16079);
#3734=VERTEX_POINT('',#16129);
#3735=VERTEX_POINT('',#16130);
#3736=VERTEX_POINT('',#16180);
#3737=VERTEX_POINT('',#16181);
#3738=VERTEX_POINT('',#16228);
#3739=VERTEX_POINT('',#16229);
#3740=VERTEX_POINT('',#16279);
#3741=VERTEX_POINT('',#16280);
#3742=VERTEX_POINT('',#16330);
#3743=VERTEX_POINT('',#16331);
#3744=VERTEX_POINT('',#16378);
#3745=VERTEX_POINT('',#16379);
#3746=VERTEX_POINT('',#16426);
#3747=VERTEX_POINT('',#16427);
#3748=VERTEX_POINT('',#16477);
#3749=VERTEX_POINT('',#16478);
#3750=VERTEX_POINT('',#16528);
#3751=VERTEX_POINT('',#16529);
#3752=VERTEX_POINT('',#16576);
#3753=VERTEX_POINT('',#16577);
#3754=VERTEX_POINT('',#16627);
#3755=VERTEX_POINT('',#16628);
#3756=VERTEX_POINT('',#16678);
#3757=VERTEX_POINT('',#16679);
#3758=VERTEX_POINT('',#16726);
#3759=VERTEX_POINT('',#16727);
#3760=VERTEX_POINT('',#16774);
#3761=VERTEX_POINT('',#16775);
#3762=VERTEX_POINT('',#16825);
#3763=VERTEX_POINT('',#16826);
#3764=VERTEX_POINT('',#16876);
#3765=VERTEX_POINT('',#16877);
#3766=VERTEX_POINT('',#16924);
#3767=VERTEX_POINT('',#16925);
#3768=VERTEX_POINT('',#16975);
#3769=VERTEX_POINT('',#16976);
#3770=VERTEX_POINT('',#17026);
#3771=VERTEX_POINT('',#17027);
#3772=VERTEX_POINT('',#17074);
#3773=VERTEX_POINT('',#17075);
#3774=VERTEX_POINT('',#17122);
#3775=VERTEX_POINT('',#17123);
#3776=VERTEX_POINT('',#17173);
#3777=VERTEX_POINT('',#17174);
#3778=VERTEX_POINT('',#17224);
#3779=VERTEX_POINT('',#17225);
#3780=VERTEX_POINT('',#17272);
#3781=VERTEX_POINT('',#17273);
#3782=VERTEX_POINT('',#17323);
#3783=VERTEX_POINT('',#17324);
#3784=VERTEX_POINT('',#17374);
#3785=VERTEX_POINT('',#17375);
#3786=VERTEX_POINT('',#17422);
#3787=VERTEX_POINT('',#17423);
#3788=VERTEX_POINT('',#17470);
#3789=VERTEX_POINT('',#17471);
#3790=VERTEX_POINT('',#17521);
#3791=VERTEX_POINT('',#17522);
#3792=VERTEX_POINT('',#17572);
#3793=VERTEX_POINT('',#17573);
#3794=VERTEX_POINT('',#17620);
#3795=VERTEX_POINT('',#17621);
#3796=VERTEX_POINT('',#17671);
#3797=VERTEX_POINT('',#17672);
#3798=VERTEX_POINT('',#17722);
#3799=VERTEX_POINT('',#17723);
#3800=VERTEX_POINT('',#17770);
#3801=VERTEX_POINT('',#17771);
#3802=VERTEX_POINT('',#17818);
#3803=VERTEX_POINT('',#17819);
#3804=VERTEX_POINT('',#17869);
#3805=VERTEX_POINT('',#17870);
#3806=VERTEX_POINT('',#17935);
#3807=VERTEX_POINT('',#17936);
#3808=VERTEX_POINT('',#18025);
#3809=VERTEX_POINT('',#18026);
#3810=VERTEX_POINT('',#18112);
#3811=VERTEX_POINT('',#18113);
#3812=VERTEX_POINT('',#18199);
#3813=VERTEX_POINT('',#18200);
#3814=VERTEX_POINT('',#18286);
#3815=VERTEX_POINT('',#18287);
#3816=VERTEX_POINT('',#18373);
#3817=VERTEX_POINT('',#18374);
#3818=VERTEX_POINT('',#18460);
#3819=VERTEX_POINT('',#18461);
#3820=VERTEX_POINT('',#18550);
#3821=VERTEX_POINT('',#18551);
#3822=VERTEX_POINT('',#18553);
#3823=VERTEX_POINT('',#18560);
#3824=VERTEX_POINT('',#18561);
#3825=VERTEX_POINT('',#18580);
#3826=VERTEX_POINT('',#18596);
#3827=VERTEX_POINT('',#18597);
#3828=VERTEX_POINT('',#18634);
#3829=VERTEX_POINT('',#18635);
#3830=VERTEX_POINT('',#18670);
#3831=VERTEX_POINT('',#18671);
#3832=VERTEX_POINT('',#18708);
#3833=VERTEX_POINT('',#18709);
#3834=VERTEX_POINT('',#18744);
#3835=VERTEX_POINT('',#18745);
#3836=VERTEX_POINT('',#18782);
#3837=VERTEX_POINT('',#18783);
#3838=VERTEX_POINT('',#18819);
#3839=VERTEX_POINT('',#18820);
#3840=VERTEX_POINT('',#18854);
#3841=VERTEX_POINT('',#18855);
#3842=VERTEX_POINT('',#18881);
#3843=VERTEX_POINT('',#18882);
#3844=VERTEX_POINT('',#18905);
#3845=VERTEX_POINT('',#18906);
#3846=VERTEX_POINT('',#18929);
#3847=VERTEX_POINT('',#18930);
#3848=VERTEX_POINT('',#18953);
#3849=VERTEX_POINT('',#18954);
#3850=VERTEX_POINT('',#18979);
#3851=VERTEX_POINT('',#18980);
#3852=VERTEX_POINT('',#19003);
#3853=VERTEX_POINT('',#19004);
#3854=VERTEX_POINT('',#19027);
#3855=VERTEX_POINT('',#19028);
#3856=VERTEX_POINT('',#19053);
#3857=VERTEX_POINT('',#19054);
#3858=VERTEX_POINT('',#19077);
#3859=VERTEX_POINT('',#19078);
#3860=VERTEX_POINT('',#19101);
#3861=VERTEX_POINT('',#19102);
#3862=VERTEX_POINT('',#19125);
#3863=VERTEX_POINT('',#19126);
#3864=VERTEX_POINT('',#19151);
#3865=VERTEX_POINT('',#19152);
#3866=VERTEX_POINT('',#19175);
#3867=VERTEX_POINT('',#19176);
#3868=VERTEX_POINT('',#19199);
#3869=VERTEX_POINT('',#19200);
#3870=VERTEX_POINT('',#19225);
#3871=VERTEX_POINT('',#19226);
#3872=VERTEX_POINT('',#19249);
#3873=VERTEX_POINT('',#19250);
#3874=VERTEX_POINT('',#19273);
#3875=VERTEX_POINT('',#19274);
#3876=VERTEX_POINT('',#19297);
#3877=VERTEX_POINT('',#19298);
#3878=VERTEX_POINT('',#19323);
#3879=VERTEX_POINT('',#19324);
#3880=VERTEX_POINT('',#19347);
#3881=VERTEX_POINT('',#19348);
#3882=VERTEX_POINT('',#19371);
#3883=VERTEX_POINT('',#19372);
#3884=VERTEX_POINT('',#19397);
#3885=VERTEX_POINT('',#19398);
#3886=VERTEX_POINT('',#19421);
#3887=VERTEX_POINT('',#19422);
#3888=VERTEX_POINT('',#19445);
#3889=VERTEX_POINT('',#19446);
#3890=VERTEX_POINT('',#19469);
#3891=VERTEX_POINT('',#19470);
#3892=VERTEX_POINT('',#19495);
#3893=VERTEX_POINT('',#19496);
#3894=VERTEX_POINT('',#19519);
#3895=VERTEX_POINT('',#19520);
#3896=VERTEX_POINT('',#19543);
#3897=VERTEX_POINT('',#19544);
#3898=VERTEX_POINT('',#19569);
#3899=VERTEX_POINT('',#19570);
#3900=VERTEX_POINT('',#19593);
#3901=VERTEX_POINT('',#19594);
#3902=VERTEX_POINT('',#19617);
#3903=VERTEX_POINT('',#19618);
#3904=VERTEX_POINT('',#19641);
#3905=VERTEX_POINT('',#19642);
#3906=VERTEX_POINT('',#19667);
#3907=VERTEX_POINT('',#19668);
#3908=VERTEX_POINT('',#19691);
#3909=VERTEX_POINT('',#19692);
#3910=VERTEX_POINT('',#19715);
#3911=VERTEX_POINT('',#19716);
#3912=VERTEX_POINT('',#19741);
#3913=VERTEX_POINT('',#19742);
#3914=VERTEX_POINT('',#19765);
#3915=VERTEX_POINT('',#19766);
#3916=VERTEX_POINT('',#19789);
#3917=VERTEX_POINT('',#19790);
#3918=VERTEX_POINT('',#19813);
#3919=VERTEX_POINT('',#19814);
#3920=VERTEX_POINT('',#19839);
#3921=VERTEX_POINT('',#19840);
#3922=VERTEX_POINT('',#19863);
#3923=VERTEX_POINT('',#19864);
#3924=VERTEX_POINT('',#19887);
#3925=VERTEX_POINT('',#19888);
#3926=VERTEX_POINT('',#19913);
#3927=VERTEX_POINT('',#19914);
#3928=VERTEX_POINT('',#19937);
#3929=VERTEX_POINT('',#19938);
#3930=VERTEX_POINT('',#19961);
#3931=VERTEX_POINT('',#19962);
#3932=VERTEX_POINT('',#19986);
#3933=VERTEX_POINT('',#19987);
#3934=VERTEX_POINT('',#20013);
#3935=VERTEX_POINT('',#20014);
#3936=VERTEX_POINT('',#20050);
#3937=VERTEX_POINT('',#20051);
#3938=VERTEX_POINT('',#20086);
#3939=VERTEX_POINT('',#20087);
#3940=VERTEX_POINT('',#20124);
#3941=VERTEX_POINT('',#20125);
#3942=VERTEX_POINT('',#20160);
#3943=VERTEX_POINT('',#20161);
#3944=VERTEX_POINT('',#20198);
#3945=VERTEX_POINT('',#20199);
#3946=VERTEX_POINT('',#20235);
#3947=VERTEX_POINT('',#20236);
#3948=VERTEX_POINT('',#22263);
#3949=VERTEX_POINT('',#22329);
#3950=VERTEX_POINT('',#22383);
#3951=VERTEX_POINT('',#24388);
#3952=VERTEX_POINT('',#24477);
#3953=VERTEX_POINT('',#24478);
#3954=VERTEX_POINT('',#24480);
#3955=VERTEX_POINT('',#24482);
#3956=VERTEX_POINT('',#24486);
#3957=VERTEX_POINT('',#24488);
#3958=VERTEX_POINT('',#24492);
#3959=VERTEX_POINT('',#24496);
#3960=VERTEX_POINT('',#24502);
#3961=VERTEX_POINT('',#24504);
#3962=VERTEX_POINT('',#24509);
#3963=VERTEX_POINT('',#24513);
#3964=VERTEX_POINT('',#24521);
#3965=VERTEX_POINT('',#24523);
#3966=VERTEX_POINT('',#24527);
#3967=VERTEX_POINT('',#24529);
#3968=VERTEX_POINT('',#24536);
#3969=VERTEX_POINT('',#24537);
#3970=VERTEX_POINT('',#24541);
#3971=VERTEX_POINT('',#24542);
#3972=VERTEX_POINT('',#24551);
#3973=VERTEX_POINT('',#24575);
#3974=VERTEX_POINT('',#24577);
#3975=VERTEX_POINT('',#24617);
#3976=VERTEX_POINT('',#24619);
#3977=VERTEX_POINT('',#24623);
#3978=VERTEX_POINT('',#24625);
#3979=VERTEX_POINT('',#24632);
#3980=VERTEX_POINT('',#24634);
#3981=VERTEX_POINT('',#24638);
#3982=VERTEX_POINT('',#24639);
#3983=VERTEX_POINT('',#24643);
#3984=VERTEX_POINT('',#24644);
#3985=VERTEX_POINT('',#24651);
#3986=VERTEX_POINT('',#24669);
#3987=VERTEX_POINT('',#24671);
#3988=VERTEX_POINT('',#24711);
#3989=VERTEX_POINT('',#24712);
#3990=VERTEX_POINT('',#24714);
#3991=VERTEX_POINT('',#24716);
#3992=VERTEX_POINT('',#24718);
#3993=VERTEX_POINT('',#24720);
#3994=VERTEX_POINT('',#24724);
#3995=VERTEX_POINT('',#24726);
#3996=VERTEX_POINT('',#24730);
#3997=VERTEX_POINT('',#24732);
#3998=VERTEX_POINT('',#24734);
#3999=VERTEX_POINT('',#24736);
#4000=VERTEX_POINT('',#24740);
#4001=VERTEX_POINT('',#24744);
#4002=VERTEX_POINT('',#24756);
#4003=VERTEX_POINT('',#24758);
#4004=VERTEX_POINT('',#24762);
#4005=VERTEX_POINT('',#24764);
#4006=VERTEX_POINT('',#24771);
#4007=VERTEX_POINT('',#24773);
#4008=VERTEX_POINT('',#24777);
#4009=VERTEX_POINT('',#24779);
#4010=VERTEX_POINT('',#24786);
#4011=VERTEX_POINT('',#24787);
#4012=VERTEX_POINT('',#24789);
#4013=VERTEX_POINT('',#24791);
#4014=VERTEX_POINT('',#24793);
#4015=VERTEX_POINT('',#24795);
#4016=VERTEX_POINT('',#24797);
#4017=VERTEX_POINT('',#24799);
#4018=VERTEX_POINT('',#24803);
#4019=VERTEX_POINT('',#24805);
#4020=VERTEX_POINT('',#24809);
#4021=VERTEX_POINT('',#24813);
#4022=VERTEX_POINT('',#24817);
#4023=VERTEX_POINT('',#24821);
#4024=VERTEX_POINT('',#24822);
#4025=VERTEX_POINT('',#24825);
#4026=VERTEX_POINT('',#24837);
#4027=VERTEX_POINT('',#24838);
#4028=VERTEX_POINT('',#24840);
#4029=VERTEX_POINT('',#24842);
#4030=VERTEX_POINT('',#24846);
#4031=VERTEX_POINT('',#24848);
#4032=VERTEX_POINT('',#24852);
#4033=VERTEX_POINT('',#24854);
#4034=VERTEX_POINT('',#24858);
#4035=VERTEX_POINT('',#24860);
#4036=VERTEX_POINT('',#24864);
#4037=VERTEX_POINT('',#24866);
#4038=VERTEX_POINT('',#24874);
#4039=VERTEX_POINT('',#24877);
#4040=VERTEX_POINT('',#24881);
#4041=VERTEX_POINT('',#24885);
#4042=VERTEX_POINT('',#24891);
#4043=VERTEX_POINT('',#24893);
#4044=VERTEX_POINT('',#24897);
#4045=VERTEX_POINT('',#24899);
#4046=VERTEX_POINT('',#24906);
#4047=VERTEX_POINT('',#24909);
#4048=VERTEX_POINT('',#24913);
#4049=VERTEX_POINT('',#24917);
#4050=VERTEX_POINT('',#24921);
#4051=VERTEX_POINT('',#24924);
#4052=VERTEX_POINT('',#24928);
#4053=VERTEX_POINT('',#24932);
#4054=VERTEX_POINT('',#24937);
#4055=VERTEX_POINT('',#24938);
#4056=VERTEX_POINT('',#24940);
#4057=VERTEX_POINT('',#24942);
#4058=VERTEX_POINT('',#24946);
#4059=VERTEX_POINT('',#24948);
#4060=VERTEX_POINT('',#24952);
#4061=VERTEX_POINT('',#24954);
#4062=VERTEX_POINT('',#24958);
#4063=VERTEX_POINT('',#24960);
#4064=VERTEX_POINT('',#24964);
#4065=VERTEX_POINT('',#24966);
#4066=EDGE_CURVE('',#3333,#3333,#3078,.T.);
#4067=EDGE_CURVE('',#3333,#3334,#2062,.T.);
#4068=EDGE_CURVE('',#3334,#3334,#3079,.T.);
#4069=EDGE_CURVE('',#3335,#3335,#3080,.T.);
#4070=EDGE_CURVE('',#3335,#3336,#2063,.T.);
#4071=EDGE_CURVE('',#3336,#3336,#3081,.T.);
#4072=EDGE_CURVE('',#3337,#3337,#3082,.T.);
#4073=EDGE_CURVE('',#3337,#3338,#2064,.T.);
#4074=EDGE_CURVE('',#3338,#3338,#3083,.T.);
#4075=EDGE_CURVE('',#3339,#3339,#3084,.T.);
#4076=EDGE_CURVE('',#3339,#3340,#2065,.T.);
#4077=EDGE_CURVE('',#3340,#3340,#3085,.T.);
#4078=EDGE_CURVE('',#3341,#3341,#3086,.T.);
#4079=EDGE_CURVE('',#3341,#3342,#2066,.T.);
#4080=EDGE_CURVE('',#3342,#3342,#3087,.T.);
#4081=EDGE_CURVE('',#3343,#3343,#3088,.T.);
#4082=EDGE_CURVE('',#3343,#3344,#2067,.T.);
#4083=EDGE_CURVE('',#3344,#3344,#3089,.T.);
#4084=EDGE_CURVE('',#3345,#3345,#3090,.T.);
#4085=EDGE_CURVE('',#3345,#3346,#2068,.T.);
#4086=EDGE_CURVE('',#3346,#3346,#3091,.T.);
#4087=EDGE_CURVE('',#3347,#3348,#2069,.T.);
#4088=EDGE_CURVE('',#3348,#3349,#2070,.T.);
#4089=EDGE_CURVE('',#3350,#3349,#2071,.T.);
#4090=EDGE_CURVE('',#3347,#3350,#2072,.T.);
#4091=EDGE_CURVE('',#3351,#3347,#2073,.T.);
#4092=EDGE_CURVE('',#3352,#3350,#2074,.T.);
#4093=EDGE_CURVE('',#3351,#3352,#2075,.T.);
#4094=EDGE_CURVE('',#3353,#3351,#2076,.T.);
#4095=EDGE_CURVE('',#3354,#3352,#2077,.T.);
#4096=EDGE_CURVE('',#3353,#3354,#2078,.T.);
#4097=EDGE_CURVE('',#3348,#3353,#2079,.T.);
#4098=EDGE_CURVE('',#3349,#3354,#2080,.T.);
#4099=EDGE_CURVE('',#3355,#3355,#3092,.T.);
#4100=EDGE_CURVE('',#3355,#3356,#2081,.T.);
#4101=EDGE_CURVE('',#3356,#3356,#3093,.T.);
#4102=EDGE_CURVE('',#3357,#3357,#3094,.T.);
#4103=EDGE_CURVE('',#3357,#3358,#2082,.T.);
#4104=EDGE_CURVE('',#3358,#3358,#3095,.T.);
#4105=EDGE_CURVE('',#3359,#3359,#3096,.T.);
#4106=EDGE_CURVE('',#3359,#3360,#2083,.T.);
#4107=EDGE_CURVE('',#3360,#3360,#3097,.T.);
#4108=EDGE_CURVE('',#3361,#3362,#2084,.T.);
#4109=EDGE_CURVE('',#3362,#3363,#2085,.T.);
#4110=EDGE_CURVE('',#3364,#3363,#2086,.T.);
#4111=EDGE_CURVE('',#3361,#3364,#2087,.T.);
#4112=EDGE_CURVE('',#3365,#3361,#2088,.T.);
#4113=EDGE_CURVE('',#3366,#3364,#2089,.T.);
#4114=EDGE_CURVE('',#3365,#3366,#2090,.T.);
#4115=EDGE_CURVE('',#3367,#3365,#2091,.T.);
#4116=EDGE_CURVE('',#3368,#3366,#2092,.T.);
#4117=EDGE_CURVE('',#3367,#3368,#2093,.T.);
#4118=EDGE_CURVE('',#3362,#3367,#2094,.T.);
#4119=EDGE_CURVE('',#3363,#3368,#2095,.T.);
#4120=EDGE_CURVE('',#3369,#3369,#3098,.T.);
#4121=EDGE_CURVE('',#3369,#3370,#2096,.T.);
#4122=EDGE_CURVE('',#3370,#3370,#3099,.T.);
#4123=EDGE_CURVE('',#3371,#3371,#3100,.T.);
#4124=EDGE_CURVE('',#3371,#3372,#2097,.T.);
#4125=EDGE_CURVE('',#3372,#3372,#3101,.T.);
#4126=EDGE_CURVE('',#3373,#3373,#3102,.T.);
#4127=EDGE_CURVE('',#3373,#3374,#2098,.T.);
#4128=EDGE_CURVE('',#3374,#3374,#3103,.T.);
#4129=EDGE_CURVE('',#3375,#3375,#3104,.T.);
#4130=EDGE_CURVE('',#3375,#3376,#2099,.T.);
#4131=EDGE_CURVE('',#3376,#3376,#3105,.T.);
#4132=EDGE_CURVE('',#3377,#3378,#2100,.T.);
#4133=EDGE_CURVE('',#3378,#3379,#2101,.T.);
#4134=EDGE_CURVE('',#3380,#3379,#2102,.T.);
#4135=EDGE_CURVE('',#3377,#3380,#2103,.T.);
#4136=EDGE_CURVE('',#3381,#3377,#2104,.T.);
#4137=EDGE_CURVE('',#3382,#3380,#2105,.T.);
#4138=EDGE_CURVE('',#3381,#3382,#2106,.T.);
#4139=EDGE_CURVE('',#3383,#3381,#2107,.T.);
#4140=EDGE_CURVE('',#3384,#3382,#2108,.T.);
#4141=EDGE_CURVE('',#3383,#3384,#2109,.T.);
#4142=EDGE_CURVE('',#3378,#3383,#2110,.T.);
#4143=EDGE_CURVE('',#3379,#3384,#2111,.T.);
#4144=EDGE_CURVE('',#3385,#3385,#3106,.T.);
#4145=EDGE_CURVE('',#3385,#3386,#2112,.T.);
#4146=EDGE_CURVE('',#3386,#3386,#3107,.T.);
#4147=EDGE_CURVE('',#3387,#3387,#3108,.T.);
#4148=EDGE_CURVE('',#3387,#3388,#2113,.T.);
#4149=EDGE_CURVE('',#3388,#3388,#3109,.T.);
#4150=EDGE_CURVE('',#3389,#3389,#3110,.T.);
#4151=EDGE_CURVE('',#3389,#3390,#2114,.T.);
#4152=EDGE_CURVE('',#3390,#3390,#3111,.T.);
#4153=EDGE_CURVE('',#3391,#3391,#3112,.T.);
#4154=EDGE_CURVE('',#3391,#3392,#2115,.T.);
#4155=EDGE_CURVE('',#3392,#3392,#3113,.T.);
#4156=EDGE_CURVE('',#3393,#3393,#3114,.T.);
#4157=EDGE_CURVE('',#3394,#3394,#3115,.T.);
#4158=EDGE_CURVE('',#3394,#3393,#2116,.T.);
#4159=EDGE_CURVE('',#3395,#3395,#3116,.T.);
#4160=EDGE_CURVE('',#3395,#3396,#2117,.T.);
#4161=EDGE_CURVE('',#3396,#3396,#3117,.T.);
#4162=EDGE_CURVE('',#3397,#3397,#3118,.T.);
#4163=EDGE_CURVE('',#3397,#3398,#2118,.T.);
#4164=EDGE_CURVE('',#3398,#3398,#3119,.T.);
#4165=EDGE_CURVE('',#3399,#3400,#2119,.T.);
#4166=EDGE_CURVE('',#3400,#3401,#2120,.T.);
#4167=EDGE_CURVE('',#3402,#3401,#2121,.T.);
#4168=EDGE_CURVE('',#3399,#3402,#2122,.T.);
#4169=EDGE_CURVE('',#3403,#3399,#2123,.T.);
#4170=EDGE_CURVE('',#3404,#3402,#2124,.T.);
#4171=EDGE_CURVE('',#3403,#3404,#2125,.T.);
#4172=EDGE_CURVE('',#3405,#3403,#2126,.T.);
#4173=EDGE_CURVE('',#3406,#3404,#2127,.T.);
#4174=EDGE_CURVE('',#3405,#3406,#2128,.T.);
#4175=EDGE_CURVE('',#3400,#3405,#2129,.T.);
#4176=EDGE_CURVE('',#3401,#3406,#2130,.T.);
#4177=EDGE_CURVE('',#3407,#3407,#3120,.T.);
#4178=EDGE_CURVE('',#3407,#3408,#2131,.T.);
#4179=EDGE_CURVE('',#3408,#3408,#3121,.T.);
#4180=EDGE_CURVE('',#3409,#3409,#3122,.T.);
#4181=EDGE_CURVE('',#3409,#3410,#2132,.T.);
#4182=EDGE_CURVE('',#3410,#3410,#3123,.T.);
#4183=EDGE_CURVE('',#3411,#3411,#3124,.T.);
#4184=EDGE_CURVE('',#3411,#3412,#2133,.T.);
#4185=EDGE_CURVE('',#3412,#3412,#3125,.T.);
#4186=EDGE_CURVE('',#3413,#3414,#2134,.T.);
#4187=EDGE_CURVE('',#3415,#3413,#2135,.T.);
#4188=EDGE_CURVE('',#3416,#3415,#2136,.T.);
#4189=EDGE_CURVE('',#3414,#3416,#2137,.T.);
#4190=EDGE_CURVE('',#3415,#3413,#3126,.T.);
#4191=EDGE_CURVE('',#3417,#3417,#3127,.T.);
#4192=EDGE_CURVE('',#3416,#3414,#3128,.T.);
#4193=EDGE_CURVE('',#3417,#3418,#2138,.T.);
#4194=EDGE_CURVE('',#3418,#3418,#3129,.T.);
#4195=EDGE_CURVE('',#3419,#3419,#3130,.T.);
#4196=EDGE_CURVE('',#3420,#3420,#3131,.T.);
#4197=EDGE_CURVE('',#3420,#3419,#2139,.T.);
#4198=EDGE_CURVE('',#3421,#3422,#2140,.T.);
#4199=EDGE_CURVE('',#3423,#3421,#2141,.T.);
#4200=EDGE_CURVE('',#3424,#3423,#2142,.T.);
#4201=EDGE_CURVE('',#3422,#3424,#2143,.T.);
#4202=EDGE_CURVE('',#3423,#3425,#2144,.T.);
#4203=EDGE_CURVE('',#3425,#3426,#2145,.T.);
#4204=EDGE_CURVE('',#3424,#3426,#2146,.T.);
#4205=EDGE_CURVE('',#3427,#3427,#3132,.T.);
#4206=EDGE_CURVE('',#3428,#3428,#3133,.T.);
#4207=EDGE_CURVE('',#3429,#3421,#2147,.T.);
#4208=EDGE_CURVE('',#3429,#3425,#2148,.T.);
#4209=EDGE_CURVE('',#3430,#3429,#2149,.T.);
#4210=EDGE_CURVE('',#3426,#3430,#2150,.T.);
#4211=EDGE_CURVE('',#3430,#3422,#2151,.T.);
#4212=EDGE_CURVE('',#3431,#3431,#3134,.T.);
#4213=EDGE_CURVE('',#3432,#3432,#3135,.T.);
#4214=EDGE_CURVE('',#3433,#3433,#3136,.T.);
#4215=EDGE_CURVE('',#3433,#3432,#2152,.T.);
#4216=EDGE_CURVE('',#3434,#3434,#3137,.T.);
#4217=EDGE_CURVE('',#3435,#3435,#3138,.T.);
#4218=EDGE_CURVE('',#3435,#3431,#2153,.T.);
#4219=EDGE_CURVE('',#3436,#3436,#3139,.T.);
#4220=EDGE_CURVE('',#3428,#3434,#2154,.T.);
#4221=EDGE_CURVE('',#3427,#3436,#2155,.T.);
#4222=EDGE_CURVE('',#3437,#3438,#2156,.T.);
#4223=EDGE_CURVE('',#3438,#3439,#2157,.T.);
#4224=EDGE_CURVE('',#3439,#3440,#2158,.T.);
#4225=EDGE_CURVE('',#3437,#3440,#2159,.T.);
#4226=EDGE_CURVE('',#3438,#3441,#2160,.T.);
#4227=EDGE_CURVE('',#3441,#3442,#2161,.T.);
#4228=EDGE_CURVE('',#3442,#3439,#2162,.T.);
#4229=EDGE_CURVE('',#3441,#3443,#2163,.T.);
#4230=EDGE_CURVE('',#3443,#3444,#2164,.T.);
#4231=EDGE_CURVE('',#3444,#3442,#2165,.T.);
#4232=EDGE_CURVE('',#3443,#3445,#2166,.T.);
#4233=EDGE_CURVE('',#3445,#3446,#2167,.T.);
#4234=EDGE_CURVE('',#3446,#3444,#2168,.T.);
#4235=EDGE_CURVE('',#3445,#3447,#2169,.T.);
#4236=EDGE_CURVE('',#3447,#3448,#2170,.T.);
#4237=EDGE_CURVE('',#3448,#3446,#2171,.T.);
#4238=EDGE_CURVE('',#3447,#3437,#2172,.T.);
#4239=EDGE_CURVE('',#3440,#3448,#2173,.T.);
#4240=EDGE_CURVE('',#3449,#3449,#3140,.T.);
#4241=EDGE_CURVE('',#3450,#3450,#3141,.T.);
#4242=EDGE_CURVE('',#3451,#3451,#3142,.T.);
#4243=EDGE_CURVE('',#3451,#3450,#2174,.T.);
#4244=EDGE_CURVE('',#3452,#3452,#3143,.T.);
#4245=EDGE_CURVE('',#3452,#3451,#2175,.T.);
#4246=EDGE_CURVE('',#3453,#3453,#3144,.T.);
#4247=EDGE_CURVE('',#3453,#3452,#2176,.T.);
#4248=EDGE_CURVE('',#3454,#3454,#3145,.T.);
#4249=EDGE_CURVE('',#3455,#3455,#3146,.F.);
#4250=EDGE_CURVE('',#3455,#3454,#2177,.T.);
#4251=EDGE_CURVE('',#3449,#3455,#2178,.T.);
#4252=EDGE_CURVE('',#3456,#3457,#3147,.T.);
#4253=EDGE_CURVE('',#3457,#3456,#3148,.T.);
#4254=EDGE_CURVE('',#3457,#3458,#3149,.T.);
#4255=EDGE_CURVE('',#3459,#3458,#3150,.T.);
#4256=EDGE_CURVE('',#3458,#3459,#3151,.T.);
#4257=EDGE_CURVE('',#3459,#3460,#2179,.T.);
#4258=EDGE_CURVE('',#3460,#3460,#3152,.T.);
#4259=EDGE_CURVE('',#3461,#3461,#3153,.T.);
#4260=EDGE_CURVE('',#3461,#3462,#2180,.T.);
#4261=EDGE_CURVE('',#3462,#3462,#3154,.T.);
#4262=EDGE_CURVE('',#3462,#3463,#2181,.T.);
#4263=EDGE_CURVE('',#3463,#3463,#3155,.T.);
#4264=EDGE_CURVE('',#3464,#3464,#3156,.T.);
#4265=EDGE_CURVE('',#3464,#3456,#2182,.T.);
#4266=EDGE_CURVE('',#3465,#3465,#3157,.T.);
#4267=EDGE_CURVE('',#3465,#3461,#2183,.T.);
#4268=EDGE_CURVE('',#3466,#3467,#3158,.T.);
#4269=EDGE_CURVE('',#3467,#3466,#3159,.T.);
#4270=EDGE_CURVE('',#3467,#3468,#3160,.T.);
#4271=EDGE_CURVE('',#3469,#3468,#3161,.T.);
#4272=EDGE_CURVE('',#3468,#3469,#3162,.T.);
#4273=EDGE_CURVE('',#3470,#3470,#3163,.T.);
#4274=EDGE_CURVE('',#3470,#3469,#2184,.T.);
#4275=EDGE_CURVE('',#3471,#3471,#3164,.T.);
#4276=EDGE_CURVE('',#3472,#3472,#3165,.T.);
#4277=EDGE_CURVE('',#3473,#3473,#3166,.T.);
#4278=EDGE_CURVE('',#3473,#3471,#2185,.T.);
#4279=EDGE_CURVE('',#3474,#3474,#3167,.T.);
#4280=EDGE_CURVE('',#3474,#3473,#2186,.T.);
#4281=EDGE_CURVE('',#3475,#3475,#3168,.T.);
#4282=EDGE_CURVE('',#3475,#3474,#2187,.T.);
#4283=EDGE_CURVE('',#3466,#3472,#2188,.T.);
#4284=EDGE_CURVE('',#3476,#3477,#3169,.T.);
#4285=EDGE_CURVE('',#3478,#3479,#3170,.T.);
#4286=EDGE_CURVE('',#3480,#3481,#3171,.T.);
#4287=EDGE_CURVE('',#3482,#3483,#3172,.T.);
#4288=EDGE_CURVE('',#3484,#3485,#3173,.T.);
#4289=EDGE_CURVE('',#3486,#3487,#3174,.T.);
#4290=EDGE_CURVE('',#3488,#3489,#3175,.T.);
#4291=EDGE_CURVE('',#3490,#3491,#3176,.T.);
#4292=EDGE_CURVE('',#3492,#3493,#211,.T.);
#4293=EDGE_CURVE('',#3494,#3492,#3177,.T.);
#4294=EDGE_CURVE('',#3495,#3494,#212,.T.);
#4295=EDGE_CURVE('',#3493,#3495,#3178,.T.);
#4296=EDGE_CURVE('',#3496,#3494,#3179,.T.);
#4297=EDGE_CURVE('',#3496,#3497,#213,.T.);
#4298=EDGE_CURVE('',#3498,#3497,#3180,.T.);
#4299=EDGE_CURVE('',#3498,#3499,#214,.T.);
#4300=EDGE_CURVE('',#3500,#3499,#3181,.T.);
#4301=EDGE_CURVE('',#3500,#3501,#215,.T.);
#4302=EDGE_CURVE('',#3501,#3502,#2189,.T.);
#4303=EDGE_CURVE('',#3502,#3502,#3182,.T.);
#4304=EDGE_CURVE('',#3501,#3503,#216,.T.);
#4305=EDGE_CURVE('',#3504,#3503,#3183,.T.);
#4306=EDGE_CURVE('',#3504,#3505,#217,.T.);
#4307=EDGE_CURVE('',#3506,#3505,#3184,.T.);
#4308=EDGE_CURVE('',#3506,#3507,#218,.T.);
#4309=EDGE_CURVE('',#3508,#3507,#3185,.T.);
#4310=EDGE_CURVE('',#3508,#3509,#219,.T.);
#4311=EDGE_CURVE('',#3510,#3509,#3186,.T.);
#4312=EDGE_CURVE('',#3510,#3511,#220,.T.);
#4313=EDGE_CURVE('',#3495,#3511,#3187,.T.);
#4314=EDGE_CURVE('',#3492,#3512,#3188,.T.);
#4315=EDGE_CURVE('',#3512,#3496,#3189,.T.);
#4316=EDGE_CURVE('',#3513,#3512,#221,.T.);
#4317=EDGE_CURVE('',#3497,#3513,#3190,.T.);
#4318=EDGE_CURVE('',#3513,#3514,#3191,.T.);
#4319=EDGE_CURVE('',#3514,#3498,#3192,.T.);
#4320=EDGE_CURVE('',#3515,#3514,#222,.T.);
#4321=EDGE_CURVE('',#3499,#3515,#3193,.T.);
#4322=EDGE_CURVE('',#3515,#3516,#3194,.T.);
#4323=EDGE_CURVE('',#3516,#3500,#3195,.T.);
#4324=EDGE_CURVE('',#3517,#3518,#223,.T.);
#4325=EDGE_CURVE('',#3503,#3517,#3196,.T.);
#4326=EDGE_CURVE('',#3518,#3516,#224,.T.);
#4327=EDGE_CURVE('',#3517,#3519,#3197,.T.);
#4328=EDGE_CURVE('',#3519,#3504,#3198,.T.);
#4329=EDGE_CURVE('',#3520,#3519,#225,.T.);
#4330=EDGE_CURVE('',#3505,#3520,#3199,.T.);
#4331=EDGE_CURVE('',#3520,#3521,#3200,.T.);
#4332=EDGE_CURVE('',#3521,#3506,#3201,.T.);
#4333=EDGE_CURVE('',#3522,#3521,#226,.T.);
#4334=EDGE_CURVE('',#3507,#3522,#3202,.T.);
#4335=EDGE_CURVE('',#3522,#3523,#3203,.T.);
#4336=EDGE_CURVE('',#3523,#3508,#3204,.T.);
#4337=EDGE_CURVE('',#3524,#3523,#227,.T.);
#4338=EDGE_CURVE('',#3509,#3524,#3205,.T.);
#4339=EDGE_CURVE('',#3525,#3525,#3206,.T.);
#4340=EDGE_CURVE('',#3525,#3518,#2190,.T.);
#4341=EDGE_CURVE('',#3526,#3493,#3207,.T.);
#4342=EDGE_CURVE('',#3526,#3527,#228,.T.);
#4343=EDGE_CURVE('',#3524,#3527,#3208,.T.);
#4344=EDGE_CURVE('',#3511,#3526,#3209,.T.);
#4345=EDGE_CURVE('',#3527,#3510,#3210,.T.);
#4346=EDGE_CURVE('',#3528,#3528,#3211,.T.);
#4347=EDGE_CURVE('',#3529,#3529,#3212,.T.);
#4348=EDGE_CURVE('',#3530,#3530,#3213,.T.);
#4349=EDGE_CURVE('',#3530,#3528,#2191,.T.);
#4350=EDGE_CURVE('',#3531,#3531,#3214,.T.);
#4351=EDGE_CURVE('',#3531,#3529,#2192,.T.);
#4352=EDGE_CURVE('',#3532,#3532,#3215,.T.);
#4353=EDGE_CURVE('',#3533,#3533,#3216,.T.);
#4354=EDGE_CURVE('',#3534,#3534,#3217,.T.);
#4355=EDGE_CURVE('',#3534,#3532,#2193,.T.);
#4356=EDGE_CURVE('',#3535,#3535,#3218,.T.);
#4357=EDGE_CURVE('',#3535,#3533,#2194,.T.);
#4358=EDGE_CURVE('',#3536,#3536,#3219,.T.);
#4359=EDGE_CURVE('',#3536,#3537,#2195,.T.);
#4360=EDGE_CURVE('',#3537,#3537,#3220,.T.);
#4361=EDGE_CURVE('',#3538,#3538,#3221,.T.);
#4362=EDGE_CURVE('',#3538,#3539,#2196,.T.);
#4363=EDGE_CURVE('',#3539,#3539,#3222,.T.);
#4364=EDGE_CURVE('',#3540,#3540,#3223,.T.);
#4365=EDGE_CURVE('',#3540,#3541,#2197,.T.);
#4366=EDGE_CURVE('',#3541,#3541,#3224,.T.);
#4367=EDGE_CURVE('',#3542,#3542,#3225,.T.);
#4368=EDGE_CURVE('',#3542,#3543,#2198,.T.);
#4369=EDGE_CURVE('',#3543,#3543,#3226,.T.);
#4370=EDGE_CURVE('',#3544,#3544,#3227,.T.);
#4371=EDGE_CURVE('',#3544,#3545,#2199,.T.);
#4372=EDGE_CURVE('',#3545,#3545,#3228,.T.);
#4373=EDGE_CURVE('',#3546,#3546,#3229,.T.);
#4374=EDGE_CURVE('',#3546,#3547,#2200,.T.);
#4375=EDGE_CURVE('',#3547,#3547,#3230,.T.);
#4376=EDGE_CURVE('',#3548,#3548,#3231,.T.);
#4377=EDGE_CURVE('',#3549,#3549,#3232,.T.);
#4378=EDGE_CURVE('',#3549,#3548,#2201,.T.);
#4379=EDGE_CURVE('',#3550,#3550,#3233,.T.);
#4380=EDGE_CURVE('',#3550,#3551,#2202,.T.);
#4381=EDGE_CURVE('',#3551,#3551,#3234,.T.);
#4382=EDGE_CURVE('',#3552,#3552,#3235,.T.);
#4383=EDGE_CURVE('',#3553,#3553,#3236,.T.);
#4384=EDGE_CURVE('',#3553,#3552,#2203,.T.);
#4385=EDGE_CURVE('',#3554,#3554,#3237,.T.);
#4386=EDGE_CURVE('',#3554,#3555,#2204,.T.);
#4387=EDGE_CURVE('',#3555,#3555,#3238,.T.);
#4388=EDGE_CURVE('',#3556,#3557,#2205,.T.);
#4389=EDGE_CURVE('',#3558,#3556,#2206,.T.);
#4390=EDGE_CURVE('',#3559,#3558,#2207,.T.);
#4391=EDGE_CURVE('',#3557,#3559,#2208,.T.);
#4392=EDGE_CURVE('',#3560,#3556,#2209,.T.);
#4393=EDGE_CURVE('',#3561,#3560,#2210,.T.);
#4394=EDGE_CURVE('',#3558,#3561,#2211,.T.);
#4395=EDGE_CURVE('',#3562,#3560,#2212,.T.);
#4396=EDGE_CURVE('',#3563,#3562,#2213,.T.);
#4397=EDGE_CURVE('',#3561,#3563,#2214,.T.);
#4398=EDGE_CURVE('',#3557,#3564,#2215,.T.);
#4399=EDGE_CURVE('',#3564,#3565,#2216,.T.);
#4400=EDGE_CURVE('',#3566,#3565,#2217,.T.);
#4401=EDGE_CURVE('',#3567,#3566,#2218,.T.);
#4402=EDGE_CURVE('',#3567,#3562,#2219,.T.);
#4403=EDGE_CURVE('',#3568,#3559,#2220,.T.);
#4404=EDGE_CURVE('',#3564,#3568,#2221,.T.);
#4405=EDGE_CURVE('',#3568,#3569,#2222,.T.);
#4406=EDGE_CURVE('',#3565,#3569,#2223,.T.);
#4407=EDGE_CURVE('',#3570,#3567,#2224,.T.);
#4408=EDGE_CURVE('',#3571,#3566,#2225,.T.);
#4409=EDGE_CURVE('',#3570,#3571,#2226,.T.);
#4410=EDGE_CURVE('',#3563,#3570,#2227,.T.);
#4411=EDGE_CURVE('',#3569,#3571,#2228,.T.);
#4412=EDGE_CURVE('',#3572,#3573,#2229,.T.);
#4413=EDGE_CURVE('',#3573,#3574,#2230,.T.);
#4414=EDGE_CURVE('',#3575,#3574,#2231,.T.);
#4415=EDGE_CURVE('',#3572,#3575,#2232,.T.);
#4416=EDGE_CURVE('',#3576,#3572,#2233,.T.);
#4417=EDGE_CURVE('',#3577,#3575,#2234,.T.);
#4418=EDGE_CURVE('',#3576,#3577,#2235,.T.);
#4419=EDGE_CURVE('',#3578,#3576,#2236,.T.);
#4420=EDGE_CURVE('',#3579,#3577,#2237,.T.);
#4421=EDGE_CURVE('',#3578,#3579,#2238,.T.);
#4422=EDGE_CURVE('',#3573,#3578,#2239,.T.);
#4423=EDGE_CURVE('',#3574,#3579,#2240,.T.);
#4424=EDGE_CURVE('',#3580,#3581,#2241,.T.);
#4425=EDGE_CURVE('',#3582,#3580,#2242,.T.);
#4426=EDGE_CURVE('',#3583,#3582,#2243,.T.);
#4427=EDGE_CURVE('',#3581,#3583,#2244,.T.);
#4428=EDGE_CURVE('',#3582,#3584,#2245,.T.);
#4429=EDGE_CURVE('',#3584,#3585,#2246,.T.);
#4430=EDGE_CURVE('',#3583,#3585,#2247,.T.);
#4431=EDGE_CURVE('',#3586,#3586,#3239,.T.);
#4432=EDGE_CURVE('',#3587,#3587,#3240,.T.);
#4433=EDGE_CURVE('',#3588,#3580,#2248,.T.);
#4434=EDGE_CURVE('',#3588,#3584,#2249,.T.);
#4435=EDGE_CURVE('',#3589,#3588,#2250,.T.);
#4436=EDGE_CURVE('',#3585,#3589,#2251,.T.);
#4437=EDGE_CURVE('',#3589,#3581,#2252,.T.);
#4438=EDGE_CURVE('',#3590,#3590,#3241,.T.);
#4439=EDGE_CURVE('',#3591,#3591,#3242,.T.);
#4440=EDGE_CURVE('',#3587,#3592,#2253,.T.);
#4441=EDGE_CURVE('',#3592,#3592,#3243,.T.);
#4442=EDGE_CURVE('',#3593,#3593,#3244,.T.);
#4443=EDGE_CURVE('',#3586,#3594,#2254,.T.);
#4444=EDGE_CURVE('',#3594,#3594,#3245,.T.);
#4445=EDGE_CURVE('',#3595,#3595,#3246,.T.);
#4446=EDGE_CURVE('',#3593,#3591,#2255,.T.);
#4447=EDGE_CURVE('',#3595,#3590,#2256,.T.);
#4448=EDGE_CURVE('',#3596,#3597,#2257,.T.);
#4449=EDGE_CURVE('',#3597,#3598,#229,.T.);
#4450=EDGE_CURVE('',#3598,#3599,#3247,.F.);
#4451=EDGE_CURVE('',#3599,#3596,#230,.T.);
#4452=EDGE_CURVE('',#3600,#3601,#2258,.T.);
#4453=EDGE_CURVE('',#3601,#3597,#231,.T.);
#4454=EDGE_CURVE('',#3596,#3600,#232,.T.);
#4455=EDGE_CURVE('',#3602,#3603,#2259,.T.);
#4456=EDGE_CURVE('',#3603,#3601,#233,.T.);
#4457=EDGE_CURVE('',#3600,#3602,#234,.T.);
#4458=EDGE_CURVE('',#3604,#3605,#2260,.T.);
#4459=EDGE_CURVE('',#3605,#3603,#235,.T.);
#4460=EDGE_CURVE('',#3602,#3604,#236,.T.);
#4461=EDGE_CURVE('',#3606,#3607,#2261,.T.);
#4462=EDGE_CURVE('',#3607,#3605,#237,.T.);
#4463=EDGE_CURVE('',#3604,#3606,#238,.T.);
#4464=EDGE_CURVE('',#3608,#3609,#2262,.T.);
#4465=EDGE_CURVE('',#3609,#3607,#239,.T.);
#4466=EDGE_CURVE('',#3606,#3608,#240,.T.);
#4467=EDGE_CURVE('',#3610,#3611,#2263,.T.);
#4468=EDGE_CURVE('',#3611,#3609,#241,.T.);
#4469=EDGE_CURVE('',#3608,#3610,#242,.T.);
#4470=EDGE_CURVE('',#3612,#3613,#2264,.T.);
#4471=EDGE_CURVE('',#3613,#3611,#243,.T.);
#4472=EDGE_CURVE('',#3610,#3612,#244,.T.);
#4473=EDGE_CURVE('',#3614,#3615,#2265,.T.);
#4474=EDGE_CURVE('',#3616,#3614,#3248,.F.);
#4475=EDGE_CURVE('',#3616,#3615,#245,.T.);
#4476=EDGE_CURVE('',#3617,#3618,#2266,.T.);
#4477=EDGE_CURVE('',#3618,#3619,#246,.T.);
#4478=EDGE_CURVE('',#3620,#3619,#3249,.T.);
#4479=EDGE_CURVE('',#3617,#3620,#247,.T.);
#4480=EDGE_CURVE('',#3621,#3622,#2267,.T.);
#4481=EDGE_CURVE('',#3622,#3618,#248,.T.);
#4482=EDGE_CURVE('',#3621,#3617,#249,.T.);
#4483=EDGE_CURVE('',#3623,#3624,#2268,.T.);
#4484=EDGE_CURVE('',#3624,#3622,#250,.T.);
#4485=EDGE_CURVE('',#3623,#3621,#251,.T.);
#4486=EDGE_CURVE('',#3625,#3626,#2269,.T.);
#4487=EDGE_CURVE('',#3626,#3624,#252,.T.);
#4488=EDGE_CURVE('',#3625,#3623,#253,.T.);
#4489=EDGE_CURVE('',#3627,#3628,#2270,.T.);
#4490=EDGE_CURVE('',#3628,#3626,#254,.T.);
#4491=EDGE_CURVE('',#3627,#3625,#255,.T.);
#4492=EDGE_CURVE('',#3629,#3630,#2271,.T.);
#4493=EDGE_CURVE('',#3630,#3628,#256,.T.);
#4494=EDGE_CURVE('',#3629,#3627,#257,.T.);
#4495=EDGE_CURVE('',#3631,#3632,#2272,.T.);
#4496=EDGE_CURVE('',#3632,#3630,#258,.T.);
#4497=EDGE_CURVE('',#3631,#3629,#259,.T.);
#4498=EDGE_CURVE('',#3633,#3634,#2273,.T.);
#4499=EDGE_CURVE('',#3634,#3632,#260,.T.);
#4500=EDGE_CURVE('',#3633,#3631,#261,.T.);
#4501=EDGE_CURVE('',#3635,#3636,#2274,.T.);
#4502=EDGE_CURVE('',#3637,#3635,#262,.T.);
#4503=EDGE_CURVE('',#3638,#3637,#3250,.T.);
#4504=EDGE_CURVE('',#3638,#3636,#263,.T.);
#4505=EDGE_CURVE('',#3636,#3634,#264,.T.);
#4506=EDGE_CURVE('',#3635,#3633,#265,.T.);
#4507=EDGE_CURVE('',#3619,#3616,#266,.T.);
#4508=EDGE_CURVE('',#3598,#3638,#267,.T.);
#4509=EDGE_CURVE('',#3615,#3613,#268,.T.);
#4510=EDGE_CURVE('',#3639,#3620,#269,.T.);
#4511=EDGE_CURVE('',#3612,#3639,#270,.T.);
#4512=EDGE_CURVE('',#3637,#3599,#271,.T.);
#4513=EDGE_CURVE('',#3640,#3641,#2275,.T.);
#4514=EDGE_CURVE('',#3641,#3640,#3251,.T.);
#4515=EDGE_CURVE('',#3614,#3639,#3252,.F.);
#4516=EDGE_CURVE('',#3642,#3642,#3253,.T.);
#4517=EDGE_CURVE('',#3643,#3643,#3254,.T.);
#4518=EDGE_CURVE('',#3644,#3644,#3255,.T.);
#4519=EDGE_CURVE('',#3645,#3645,#3256,.T.);
#4520=EDGE_CURVE('',#3645,#3644,#2276,.T.);
#4521=EDGE_CURVE('',#3646,#3646,#3257,.T.);
#4522=EDGE_CURVE('',#3646,#3643,#2277,.T.);
#4523=EDGE_CURVE('',#3647,#3647,#3258,.T.);
#4524=EDGE_CURVE('',#3647,#3642,#2278,.T.);
#4525=EDGE_CURVE('',#3648,#3649,#2279,.T.);
#4526=EDGE_CURVE('',#3641,#3648,#2280,.T.);
#4527=EDGE_CURVE('',#3649,#3640,#2281,.T.);
#4528=EDGE_CURVE('',#3648,#3649,#3259,.T.);
#4529=EDGE_CURVE('',#3650,#3650,#3260,.T.);
#4530=EDGE_CURVE('',#3650,#3651,#2282,.T.);
#4531=EDGE_CURVE('',#3651,#3651,#3261,.T.);
#4532=EDGE_CURVE('',#3652,#3652,#3262,.T.);
#4533=EDGE_CURVE('',#3653,#3653,#3263,.T.);
#4534=EDGE_CURVE('',#3653,#3652,#2283,.T.);
#4535=EDGE_CURVE('',#3654,#3654,#3264,.T.);
#4536=EDGE_CURVE('',#3654,#3653,#2284,.T.);
#4537=EDGE_CURVE('',#3655,#3655,#3265,.T.);
#4538=EDGE_CURVE('',#3655,#3654,#2285,.T.);
#4539=EDGE_CURVE('',#3656,#3656,#3266,.T.);
#4540=EDGE_CURVE('',#3657,#3657,#3267,.F.);
#4541=EDGE_CURVE('',#3657,#3656,#2286,.T.);
#4542=EDGE_CURVE('',#3658,#3658,#3268,.F.);
#4543=EDGE_CURVE('',#3658,#3657,#2287,.T.);
#4544=EDGE_CURVE('',#3659,#3659,#3269,.T.);
#4545=EDGE_CURVE('',#3659,#3658,#2288,.T.);
#4546=EDGE_CURVE('',#3660,#3661,#2289,.T.);
#4547=EDGE_CURVE('',#3661,#3662,#2290,.T.);
#4548=EDGE_CURVE('',#3662,#3663,#2291,.T.);
#4549=EDGE_CURVE('',#3660,#3663,#2292,.T.);
#4550=EDGE_CURVE('',#3661,#3664,#2293,.T.);
#4551=EDGE_CURVE('',#3664,#3665,#2294,.T.);
#4552=EDGE_CURVE('',#3665,#3662,#2295,.T.);
#4553=EDGE_CURVE('',#3664,#3666,#2296,.T.);
#4554=EDGE_CURVE('',#3666,#3667,#2297,.T.);
#4555=EDGE_CURVE('',#3667,#3665,#2298,.T.);
#4556=EDGE_CURVE('',#3666,#3668,#2299,.T.);
#4557=EDGE_CURVE('',#3668,#3669,#2300,.T.);
#4558=EDGE_CURVE('',#3669,#3667,#2301,.T.);
#4559=EDGE_CURVE('',#3668,#3670,#2302,.T.);
#4560=EDGE_CURVE('',#3670,#3671,#2303,.T.);
#4561=EDGE_CURVE('',#3671,#3669,#2304,.T.);
#4562=EDGE_CURVE('',#3670,#3660,#2305,.T.);
#4563=EDGE_CURVE('',#3663,#3671,#2306,.T.);
#4564=EDGE_CURVE('',#3672,#3672,#3270,.T.);
#4565=EDGE_CURVE('',#3673,#3673,#3271,.T.);
#4566=EDGE_CURVE('',#3673,#3672,#2307,.T.);
#4567=EDGE_CURVE('',#3674,#3674,#3272,.T.);
#4568=EDGE_CURVE('',#3674,#3673,#2308,.T.);
#4569=EDGE_CURVE('',#3675,#3675,#3273,.T.);
#4570=EDGE_CURVE('',#3675,#3674,#2309,.T.);
#4571=EDGE_CURVE('',#3676,#3676,#3274,.T.);
#4572=EDGE_CURVE('',#3677,#3677,#3275,.F.);
#4573=EDGE_CURVE('',#3677,#3676,#2310,.T.);
#4574=EDGE_CURVE('',#3678,#3678,#3276,.F.);
#4575=EDGE_CURVE('',#3678,#3677,#2311,.T.);
#4576=EDGE_CURVE('',#3679,#3679,#3277,.T.);
#4577=EDGE_CURVE('',#3679,#3678,#2312,.T.);
#4578=EDGE_CURVE('',#3680,#3681,#2313,.T.);
#4579=EDGE_CURVE('',#3681,#3682,#2314,.T.);
#4580=EDGE_CURVE('',#3682,#3683,#2315,.T.);
#4581=EDGE_CURVE('',#3680,#3683,#2316,.T.);
#4582=EDGE_CURVE('',#3681,#3684,#2317,.T.);
#4583=EDGE_CURVE('',#3684,#3685,#2318,.T.);
#4584=EDGE_CURVE('',#3685,#3682,#2319,.T.);
#4585=EDGE_CURVE('',#3684,#3686,#2320,.T.);
#4586=EDGE_CURVE('',#3686,#3687,#2321,.T.);
#4587=EDGE_CURVE('',#3687,#3685,#2322,.T.);
#4588=EDGE_CURVE('',#3686,#3688,#2323,.T.);
#4589=EDGE_CURVE('',#3688,#3689,#2324,.T.);
#4590=EDGE_CURVE('',#3689,#3687,#2325,.T.);
#4591=EDGE_CURVE('',#3688,#3690,#2326,.T.);
#4592=EDGE_CURVE('',#3690,#3691,#2327,.T.);
#4593=EDGE_CURVE('',#3691,#3689,#2328,.T.);
#4594=EDGE_CURVE('',#3690,#3680,#2329,.T.);
#4595=EDGE_CURVE('',#3683,#3691,#2330,.T.);
#4596=EDGE_CURVE('',#3692,#3693,#2331,.T.);
#4597=EDGE_CURVE('',#3692,#3694,#272,.T.);
#4598=EDGE_CURVE('',#3694,#3695,#3278,.F.);
#4599=EDGE_CURVE('',#3695,#3693,#273,.T.);
#4600=EDGE_CURVE('',#3696,#3697,#2332,.T.);
#4601=EDGE_CURVE('',#3696,#3692,#274,.T.);
#4602=EDGE_CURVE('',#3693,#3697,#275,.T.);
#4603=EDGE_CURVE('',#3698,#3699,#2333,.T.);
#4604=EDGE_CURVE('',#3698,#3696,#276,.T.);
#4605=EDGE_CURVE('',#3697,#3699,#277,.T.);
#4606=EDGE_CURVE('',#3700,#3701,#2334,.T.);
#4607=EDGE_CURVE('',#3700,#3698,#278,.T.);
#4608=EDGE_CURVE('',#3699,#3701,#279,.T.);
#4609=EDGE_CURVE('',#3702,#3703,#2335,.T.);
#4610=EDGE_CURVE('',#3702,#3700,#280,.T.);
#4611=EDGE_CURVE('',#3701,#3703,#281,.T.);
#4612=EDGE_CURVE('',#3704,#3705,#2336,.T.);
#4613=EDGE_CURVE('',#3704,#3702,#282,.T.);
#4614=EDGE_CURVE('',#3703,#3705,#283,.T.);
#4615=EDGE_CURVE('',#3706,#3707,#2337,.T.);
#4616=EDGE_CURVE('',#3706,#3704,#284,.T.);
#4617=EDGE_CURVE('',#3705,#3707,#285,.T.);
#4618=EDGE_CURVE('',#3708,#3709,#2338,.T.);
#4619=EDGE_CURVE('',#3708,#3706,#286,.T.);
#4620=EDGE_CURVE('',#3707,#3709,#287,.T.);
#4621=EDGE_CURVE('',#3710,#3711,#2339,.T.);
#4622=EDGE_CURVE('',#3710,#3708,#288,.T.);
#4623=EDGE_CURVE('',#3709,#3711,#289,.T.);
#4624=EDGE_CURVE('',#3712,#3713,#2340,.T.);
#4625=EDGE_CURVE('',#3712,#3710,#290,.T.);
#4626=EDGE_CURVE('',#3711,#3713,#291,.T.);
#4627=EDGE_CURVE('',#3714,#3715,#2341,.T.);
#4628=EDGE_CURVE('',#3714,#3712,#292,.T.);
#4629=EDGE_CURVE('',#3713,#3715,#293,.T.);
#4630=EDGE_CURVE('',#3716,#3717,#2342,.T.);
#4631=EDGE_CURVE('',#3716,#3714,#294,.T.);
#4632=EDGE_CURVE('',#3715,#3717,#295,.T.);
#4633=EDGE_CURVE('',#3718,#3719,#2343,.T.);
#4634=EDGE_CURVE('',#3718,#3716,#296,.T.);
#4635=EDGE_CURVE('',#3717,#3719,#297,.T.);
#4636=EDGE_CURVE('',#3720,#3721,#2344,.T.);
#4637=EDGE_CURVE('',#3720,#3718,#298,.T.);
#4638=EDGE_CURVE('',#3719,#3721,#299,.T.);
#4639=EDGE_CURVE('',#3722,#3723,#2345,.T.);
#4640=EDGE_CURVE('',#3722,#3720,#300,.T.);
#4641=EDGE_CURVE('',#3721,#3723,#301,.T.);
#4642=EDGE_CURVE('',#3724,#3725,#2346,.T.);
#4643=EDGE_CURVE('',#3724,#3722,#302,.T.);
#4644=EDGE_CURVE('',#3723,#3725,#303,.T.);
#4645=EDGE_CURVE('',#3726,#3727,#2347,.T.);
#4646=EDGE_CURVE('',#3726,#3724,#304,.T.);
#4647=EDGE_CURVE('',#3725,#3727,#305,.T.);
#4648=EDGE_CURVE('',#3728,#3729,#2348,.T.);
#4649=EDGE_CURVE('',#3728,#3726,#306,.T.);
#4650=EDGE_CURVE('',#3727,#3729,#307,.T.);
#4651=EDGE_CURVE('',#3730,#3731,#2349,.T.);
#4652=EDGE_CURVE('',#3730,#3728,#308,.T.);
#4653=EDGE_CURVE('',#3729,#3731,#309,.T.);
#4654=EDGE_CURVE('',#3732,#3733,#2350,.T.);
#4655=EDGE_CURVE('',#3732,#3730,#310,.T.);
#4656=EDGE_CURVE('',#3731,#3733,#311,.T.);
#4657=EDGE_CURVE('',#3734,#3735,#2351,.T.);
#4658=EDGE_CURVE('',#3734,#3732,#312,.T.);
#4659=EDGE_CURVE('',#3733,#3735,#313,.T.);
#4660=EDGE_CURVE('',#3736,#3737,#2352,.T.);
#4661=EDGE_CURVE('',#3736,#3734,#314,.T.);
#4662=EDGE_CURVE('',#3735,#3737,#315,.T.);
#4663=EDGE_CURVE('',#3738,#3739,#2353,.T.);
#4664=EDGE_CURVE('',#3738,#3736,#316,.T.);
#4665=EDGE_CURVE('',#3737,#3739,#317,.T.);
#4666=EDGE_CURVE('',#3740,#3741,#2354,.T.);
#4667=EDGE_CURVE('',#3740,#3738,#318,.T.);
#4668=EDGE_CURVE('',#3739,#3741,#319,.T.);
#4669=EDGE_CURVE('',#3742,#3743,#2355,.T.);
#4670=EDGE_CURVE('',#3742,#3740,#320,.T.);
#4671=EDGE_CURVE('',#3741,#3743,#321,.T.);
#4672=EDGE_CURVE('',#3744,#3745,#2356,.T.);
#4673=EDGE_CURVE('',#3744,#3742,#322,.T.);
#4674=EDGE_CURVE('',#3743,#3745,#323,.T.);
#4675=EDGE_CURVE('',#3746,#3747,#2357,.T.);
#4676=EDGE_CURVE('',#3746,#3744,#324,.T.);
#4677=EDGE_CURVE('',#3745,#3747,#325,.T.);
#4678=EDGE_CURVE('',#3748,#3749,#2358,.T.);
#4679=EDGE_CURVE('',#3748,#3746,#326,.T.);
#4680=EDGE_CURVE('',#3747,#3749,#327,.T.);
#4681=EDGE_CURVE('',#3750,#3751,#2359,.T.);
#4682=EDGE_CURVE('',#3750,#3748,#328,.T.);
#4683=EDGE_CURVE('',#3749,#3751,#329,.T.);
#4684=EDGE_CURVE('',#3752,#3753,#2360,.T.);
#4685=EDGE_CURVE('',#3752,#3750,#330,.T.);
#4686=EDGE_CURVE('',#3751,#3753,#331,.T.);
#4687=EDGE_CURVE('',#3754,#3755,#2361,.T.);
#4688=EDGE_CURVE('',#3754,#3752,#332,.T.);
#4689=EDGE_CURVE('',#3753,#3755,#333,.T.);
#4690=EDGE_CURVE('',#3756,#3757,#2362,.T.);
#4691=EDGE_CURVE('',#3756,#3754,#334,.T.);
#4692=EDGE_CURVE('',#3755,#3757,#335,.T.);
#4693=EDGE_CURVE('',#3758,#3759,#2363,.T.);
#4694=EDGE_CURVE('',#3758,#3756,#336,.T.);
#4695=EDGE_CURVE('',#3757,#3759,#337,.T.);
#4696=EDGE_CURVE('',#3760,#3761,#2364,.T.);
#4697=EDGE_CURVE('',#3760,#3758,#338,.T.);
#4698=EDGE_CURVE('',#3759,#3761,#339,.T.);
#4699=EDGE_CURVE('',#3762,#3763,#2365,.T.);
#4700=EDGE_CURVE('',#3762,#3760,#340,.T.);
#4701=EDGE_CURVE('',#3761,#3763,#341,.T.);
#4702=EDGE_CURVE('',#3764,#3765,#2366,.T.);
#4703=EDGE_CURVE('',#3764,#3762,#342,.T.);
#4704=EDGE_CURVE('',#3763,#3765,#343,.T.);
#4705=EDGE_CURVE('',#3766,#3767,#2367,.T.);
#4706=EDGE_CURVE('',#3766,#3764,#344,.T.);
#4707=EDGE_CURVE('',#3765,#3767,#345,.T.);
#4708=EDGE_CURVE('',#3768,#3769,#2368,.T.);
#4709=EDGE_CURVE('',#3768,#3766,#346,.T.);
#4710=EDGE_CURVE('',#3767,#3769,#347,.T.);
#4711=EDGE_CURVE('',#3770,#3771,#2369,.T.);
#4712=EDGE_CURVE('',#3770,#3768,#348,.T.);
#4713=EDGE_CURVE('',#3769,#3771,#349,.T.);
#4714=EDGE_CURVE('',#3772,#3773,#2370,.T.);
#4715=EDGE_CURVE('',#3772,#3770,#350,.T.);
#4716=EDGE_CURVE('',#3771,#3773,#351,.T.);
#4717=EDGE_CURVE('',#3774,#3775,#2371,.T.);
#4718=EDGE_CURVE('',#3774,#3772,#352,.T.);
#4719=EDGE_CURVE('',#3773,#3775,#353,.T.);
#4720=EDGE_CURVE('',#3776,#3777,#2372,.T.);
#4721=EDGE_CURVE('',#3776,#3774,#354,.T.);
#4722=EDGE_CURVE('',#3775,#3777,#355,.T.);
#4723=EDGE_CURVE('',#3778,#3779,#2373,.T.);
#4724=EDGE_CURVE('',#3778,#3776,#356,.T.);
#4725=EDGE_CURVE('',#3777,#3779,#357,.T.);
#4726=EDGE_CURVE('',#3780,#3781,#2374,.T.);
#4727=EDGE_CURVE('',#3780,#3778,#358,.T.);
#4728=EDGE_CURVE('',#3779,#3781,#359,.T.);
#4729=EDGE_CURVE('',#3782,#3783,#2375,.T.);
#4730=EDGE_CURVE('',#3782,#3780,#360,.T.);
#4731=EDGE_CURVE('',#3781,#3783,#361,.T.);
#4732=EDGE_CURVE('',#3784,#3785,#2376,.T.);
#4733=EDGE_CURVE('',#3784,#3782,#362,.T.);
#4734=EDGE_CURVE('',#3783,#3785,#363,.T.);
#4735=EDGE_CURVE('',#3786,#3787,#2377,.T.);
#4736=EDGE_CURVE('',#3786,#3784,#364,.T.);
#4737=EDGE_CURVE('',#3785,#3787,#365,.T.);
#4738=EDGE_CURVE('',#3788,#3789,#2378,.T.);
#4739=EDGE_CURVE('',#3788,#3786,#366,.T.);
#4740=EDGE_CURVE('',#3787,#3789,#367,.T.);
#4741=EDGE_CURVE('',#3790,#3791,#2379,.T.);
#4742=EDGE_CURVE('',#3790,#3788,#368,.T.);
#4743=EDGE_CURVE('',#3789,#3791,#369,.T.);
#4744=EDGE_CURVE('',#3792,#3793,#2380,.T.);
#4745=EDGE_CURVE('',#3792,#3790,#370,.T.);
#4746=EDGE_CURVE('',#3791,#3793,#371,.T.);
#4747=EDGE_CURVE('',#3794,#3795,#2381,.T.);
#4748=EDGE_CURVE('',#3794,#3792,#372,.T.);
#4749=EDGE_CURVE('',#3793,#3795,#373,.T.);
#4750=EDGE_CURVE('',#3796,#3797,#2382,.T.);
#4751=EDGE_CURVE('',#3796,#3794,#374,.T.);
#4752=EDGE_CURVE('',#3795,#3797,#375,.T.);
#4753=EDGE_CURVE('',#3798,#3799,#2383,.T.);
#4754=EDGE_CURVE('',#3798,#3796,#376,.T.);
#4755=EDGE_CURVE('',#3797,#3799,#377,.T.);
#4756=EDGE_CURVE('',#3800,#3801,#2384,.T.);
#4757=EDGE_CURVE('',#3800,#3798,#378,.T.);
#4758=EDGE_CURVE('',#3799,#3801,#379,.T.);
#4759=EDGE_CURVE('',#3802,#3803,#2385,.T.);
#4760=EDGE_CURVE('',#3802,#3800,#380,.T.);
#4761=EDGE_CURVE('',#3801,#3803,#381,.T.);
#4762=EDGE_CURVE('',#3804,#3805,#2386,.T.);
#4763=EDGE_CURVE('',#3804,#3802,#382,.T.);
#4764=EDGE_CURVE('',#3803,#3805,#383,.T.);
#4765=EDGE_CURVE('',#3806,#3807,#2387,.T.);
#4766=EDGE_CURVE('',#3806,#3804,#384,.T.);
#4767=EDGE_CURVE('',#3805,#3807,#385,.T.);
#4768=EDGE_CURVE('',#3808,#3809,#2388,.T.);
#4769=EDGE_CURVE('',#3808,#3806,#386,.T.);
#4770=EDGE_CURVE('',#3807,#3809,#387,.T.);
#4771=EDGE_CURVE('',#3810,#3811,#2389,.T.);
#4772=EDGE_CURVE('',#3810,#3808,#388,.T.);
#4773=EDGE_CURVE('',#3809,#3811,#389,.T.);
#4774=EDGE_CURVE('',#3812,#3813,#2390,.T.);
#4775=EDGE_CURVE('',#3812,#3810,#390,.T.);
#4776=EDGE_CURVE('',#3811,#3813,#391,.T.);
#4777=EDGE_CURVE('',#3814,#3815,#2391,.T.);
#4778=EDGE_CURVE('',#3814,#3812,#392,.T.);
#4779=EDGE_CURVE('',#3813,#3815,#393,.T.);
#4780=EDGE_CURVE('',#3816,#3817,#2392,.T.);
#4781=EDGE_CURVE('',#3816,#3814,#394,.T.);
#4782=EDGE_CURVE('',#3815,#3817,#395,.T.);
#4783=EDGE_CURVE('',#3818,#3819,#2393,.T.);
#4784=EDGE_CURVE('',#3818,#3816,#396,.T.);
#4785=EDGE_CURVE('',#3817,#3819,#397,.T.);
#4786=EDGE_CURVE('',#3820,#3821,#2394,.T.);
#4787=EDGE_CURVE('',#3820,#3822,#398,.T.);
#4788=EDGE_CURVE('',#3821,#3822,#3279,.T.);
#4789=EDGE_CURVE('',#3823,#3824,#2395,.T.);
#4790=EDGE_CURVE('',#3823,#3820,#399,.T.);
#4791=EDGE_CURVE('',#3825,#3821,#3280,.T.);
#4792=EDGE_CURVE('',#3824,#3825,#400,.T.);
#4793=EDGE_CURVE('',#3826,#3827,#2396,.T.);
#4794=EDGE_CURVE('',#3826,#3823,#401,.T.);
#4795=EDGE_CURVE('',#3827,#3824,#402,.T.);
#4796=EDGE_CURVE('',#3828,#3829,#2397,.T.);
#4797=EDGE_CURVE('',#3828,#3826,#403,.T.);
#4798=EDGE_CURVE('',#3829,#3827,#404,.T.);
#4799=EDGE_CURVE('',#3830,#3831,#2398,.T.);
#4800=EDGE_CURVE('',#3830,#3828,#405,.T.);
#4801=EDGE_CURVE('',#3831,#3829,#406,.T.);
#4802=EDGE_CURVE('',#3832,#3833,#2399,.T.);
#4803=EDGE_CURVE('',#3832,#3830,#407,.T.);
#4804=EDGE_CURVE('',#3833,#3831,#408,.T.);
#4805=EDGE_CURVE('',#3834,#3835,#2400,.T.);
#4806=EDGE_CURVE('',#3834,#3832,#409,.T.);
#4807=EDGE_CURVE('',#3835,#3833,#410,.T.);
#4808=EDGE_CURVE('',#3836,#3837,#2401,.T.);
#4809=EDGE_CURVE('',#3836,#3834,#411,.T.);
#4810=EDGE_CURVE('',#3837,#3835,#412,.T.);
#4811=EDGE_CURVE('',#3838,#3839,#2402,.T.);
#4812=EDGE_CURVE('',#3838,#3836,#413,.T.);
#4813=EDGE_CURVE('',#3839,#3837,#414,.T.);
#4814=EDGE_CURVE('',#3840,#3841,#2403,.T.);
#4815=EDGE_CURVE('',#3840,#3838,#415,.T.);
#4816=EDGE_CURVE('',#3841,#3839,#416,.T.);
#4817=EDGE_CURVE('',#3842,#3843,#2404,.T.);
#4818=EDGE_CURVE('',#3842,#3840,#417,.T.);
#4819=EDGE_CURVE('',#3843,#3841,#418,.T.);
#4820=EDGE_CURVE('',#3844,#3845,#2405,.T.);
#4821=EDGE_CURVE('',#3844,#3842,#419,.T.);
#4822=EDGE_CURVE('',#3845,#3843,#420,.T.);
#4823=EDGE_CURVE('',#3846,#3847,#2406,.T.);
#4824=EDGE_CURVE('',#3846,#3844,#421,.T.);
#4825=EDGE_CURVE('',#3847,#3845,#422,.T.);
#4826=EDGE_CURVE('',#3848,#3849,#2407,.T.);
#4827=EDGE_CURVE('',#3848,#3846,#423,.T.);
#4828=EDGE_CURVE('',#3849,#3847,#424,.T.);
#4829=EDGE_CURVE('',#3850,#3851,#2408,.T.);
#4830=EDGE_CURVE('',#3850,#3848,#425,.T.);
#4831=EDGE_CURVE('',#3851,#3849,#426,.T.);
#4832=EDGE_CURVE('',#3852,#3853,#2409,.T.);
#4833=EDGE_CURVE('',#3852,#3850,#427,.T.);
#4834=EDGE_CURVE('',#3853,#3851,#428,.T.);
#4835=EDGE_CURVE('',#3854,#3855,#2410,.T.);
#4836=EDGE_CURVE('',#3854,#3852,#429,.T.);
#4837=EDGE_CURVE('',#3855,#3853,#430,.T.);
#4838=EDGE_CURVE('',#3856,#3857,#2411,.T.);
#4839=EDGE_CURVE('',#3856,#3854,#431,.T.);
#4840=EDGE_CURVE('',#3857,#3855,#432,.T.);
#4841=EDGE_CURVE('',#3858,#3859,#2412,.T.);
#4842=EDGE_CURVE('',#3858,#3856,#433,.T.);
#4843=EDGE_CURVE('',#3859,#3857,#434,.T.);
#4844=EDGE_CURVE('',#3860,#3861,#2413,.T.);
#4845=EDGE_CURVE('',#3860,#3858,#435,.T.);
#4846=EDGE_CURVE('',#3861,#3859,#436,.T.);
#4847=EDGE_CURVE('',#3862,#3863,#2414,.T.);
#4848=EDGE_CURVE('',#3862,#3860,#437,.T.);
#4849=EDGE_CURVE('',#3863,#3861,#438,.T.);
#4850=EDGE_CURVE('',#3864,#3865,#2415,.T.);
#4851=EDGE_CURVE('',#3864,#3862,#439,.T.);
#4852=EDGE_CURVE('',#3865,#3863,#440,.T.);
#4853=EDGE_CURVE('',#3866,#3867,#2416,.T.);
#4854=EDGE_CURVE('',#3866,#3864,#441,.T.);
#4855=EDGE_CURVE('',#3867,#3865,#442,.T.);
#4856=EDGE_CURVE('',#3868,#3869,#2417,.T.);
#4857=EDGE_CURVE('',#3868,#3866,#443,.T.);
#4858=EDGE_CURVE('',#3869,#3867,#444,.T.);
#4859=EDGE_CURVE('',#3870,#3871,#2418,.T.);
#4860=EDGE_CURVE('',#3870,#3868,#445,.T.);
#4861=EDGE_CURVE('',#3871,#3869,#446,.T.);
#4862=EDGE_CURVE('',#3872,#3873,#2419,.T.);
#4863=EDGE_CURVE('',#3872,#3870,#447,.T.);
#4864=EDGE_CURVE('',#3873,#3871,#448,.T.);
#4865=EDGE_CURVE('',#3874,#3875,#2420,.T.);
#4866=EDGE_CURVE('',#3874,#3872,#449,.T.);
#4867=EDGE_CURVE('',#3875,#3873,#450,.T.);
#4868=EDGE_CURVE('',#3876,#3877,#2421,.T.);
#4869=EDGE_CURVE('',#3876,#3874,#451,.T.);
#4870=EDGE_CURVE('',#3877,#3875,#452,.T.);
#4871=EDGE_CURVE('',#3878,#3879,#2422,.T.);
#4872=EDGE_CURVE('',#3878,#3876,#453,.T.);
#4873=EDGE_CURVE('',#3879,#3877,#454,.T.);
#4874=EDGE_CURVE('',#3880,#3881,#2423,.T.);
#4875=EDGE_CURVE('',#3880,#3878,#455,.T.);
#4876=EDGE_CURVE('',#3881,#3879,#456,.T.);
#4877=EDGE_CURVE('',#3882,#3883,#2424,.T.);
#4878=EDGE_CURVE('',#3882,#3880,#457,.T.);
#4879=EDGE_CURVE('',#3883,#3881,#458,.T.);
#4880=EDGE_CURVE('',#3884,#3885,#2425,.T.);
#4881=EDGE_CURVE('',#3884,#3882,#459,.T.);
#4882=EDGE_CURVE('',#3885,#3883,#460,.T.);
#4883=EDGE_CURVE('',#3886,#3887,#2426,.T.);
#4884=EDGE_CURVE('',#3886,#3884,#461,.T.);
#4885=EDGE_CURVE('',#3887,#3885,#462,.T.);
#4886=EDGE_CURVE('',#3888,#3889,#2427,.T.);
#4887=EDGE_CURVE('',#3888,#3886,#463,.T.);
#4888=EDGE_CURVE('',#3889,#3887,#464,.T.);
#4889=EDGE_CURVE('',#3890,#3891,#2428,.T.);
#4890=EDGE_CURVE('',#3890,#3888,#465,.T.);
#4891=EDGE_CURVE('',#3891,#3889,#466,.T.);
#4892=EDGE_CURVE('',#3892,#3893,#2429,.T.);
#4893=EDGE_CURVE('',#3892,#3890,#467,.T.);
#4894=EDGE_CURVE('',#3893,#3891,#468,.T.);
#4895=EDGE_CURVE('',#3894,#3895,#2430,.T.);
#4896=EDGE_CURVE('',#3894,#3892,#469,.T.);
#4897=EDGE_CURVE('',#3895,#3893,#470,.T.);
#4898=EDGE_CURVE('',#3896,#3897,#2431,.T.);
#4899=EDGE_CURVE('',#3896,#3894,#471,.T.);
#4900=EDGE_CURVE('',#3897,#3895,#472,.T.);
#4901=EDGE_CURVE('',#3898,#3899,#2432,.T.);
#4902=EDGE_CURVE('',#3898,#3896,#473,.T.);
#4903=EDGE_CURVE('',#3899,#3897,#474,.T.);
#4904=EDGE_CURVE('',#3900,#3901,#2433,.T.);
#4905=EDGE_CURVE('',#3900,#3898,#475,.T.);
#4906=EDGE_CURVE('',#3901,#3899,#476,.T.);
#4907=EDGE_CURVE('',#3902,#3903,#2434,.T.);
#4908=EDGE_CURVE('',#3902,#3900,#477,.T.);
#4909=EDGE_CURVE('',#3903,#3901,#478,.T.);
#4910=EDGE_CURVE('',#3904,#3905,#2435,.T.);
#4911=EDGE_CURVE('',#3904,#3902,#479,.T.);
#4912=EDGE_CURVE('',#3905,#3903,#480,.T.);
#4913=EDGE_CURVE('',#3906,#3907,#2436,.T.);
#4914=EDGE_CURVE('',#3906,#3904,#481,.T.);
#4915=EDGE_CURVE('',#3907,#3905,#482,.T.);
#4916=EDGE_CURVE('',#3908,#3909,#2437,.T.);
#4917=EDGE_CURVE('',#3908,#3906,#483,.T.);
#4918=EDGE_CURVE('',#3909,#3907,#484,.T.);
#4919=EDGE_CURVE('',#3910,#3911,#2438,.T.);
#4920=EDGE_CURVE('',#3910,#3908,#485,.T.);
#4921=EDGE_CURVE('',#3911,#3909,#486,.T.);
#4922=EDGE_CURVE('',#3912,#3913,#2439,.T.);
#4923=EDGE_CURVE('',#3912,#3910,#487,.T.);
#4924=EDGE_CURVE('',#3913,#3911,#488,.T.);
#4925=EDGE_CURVE('',#3914,#3915,#2440,.T.);
#4926=EDGE_CURVE('',#3914,#3912,#489,.T.);
#4927=EDGE_CURVE('',#3915,#3913,#490,.T.);
#4928=EDGE_CURVE('',#3916,#3917,#2441,.T.);
#4929=EDGE_CURVE('',#3916,#3914,#491,.T.);
#4930=EDGE_CURVE('',#3917,#3915,#492,.T.);
#4931=EDGE_CURVE('',#3918,#3919,#2442,.T.);
#4932=EDGE_CURVE('',#3918,#3916,#493,.T.);
#4933=EDGE_CURVE('',#3919,#3917,#494,.T.);
#4934=EDGE_CURVE('',#3920,#3921,#2443,.T.);
#4935=EDGE_CURVE('',#3920,#3918,#495,.T.);
#4936=EDGE_CURVE('',#3921,#3919,#496,.T.);
#4937=EDGE_CURVE('',#3922,#3923,#2444,.T.);
#4938=EDGE_CURVE('',#3922,#3920,#497,.T.);
#4939=EDGE_CURVE('',#3923,#3921,#498,.T.);
#4940=EDGE_CURVE('',#3924,#3925,#2445,.T.);
#4941=EDGE_CURVE('',#3924,#3922,#499,.T.);
#4942=EDGE_CURVE('',#3925,#3923,#500,.T.);
#4943=EDGE_CURVE('',#3926,#3927,#2446,.T.);
#4944=EDGE_CURVE('',#3926,#3924,#501,.T.);
#4945=EDGE_CURVE('',#3927,#3925,#502,.T.);
#4946=EDGE_CURVE('',#3928,#3929,#2447,.T.);
#4947=EDGE_CURVE('',#3928,#3926,#503,.T.);
#4948=EDGE_CURVE('',#3929,#3927,#504,.T.);
#4949=EDGE_CURVE('',#3930,#3931,#2448,.T.);
#4950=EDGE_CURVE('',#3930,#3928,#505,.T.);
#4951=EDGE_CURVE('',#3931,#3929,#506,.T.);
#4952=EDGE_CURVE('',#3932,#3933,#2449,.T.);
#4953=EDGE_CURVE('',#3932,#3930,#507,.T.);
#4954=EDGE_CURVE('',#3933,#3931,#508,.T.);
#4955=EDGE_CURVE('',#3934,#3935,#2450,.T.);
#4956=EDGE_CURVE('',#3934,#3932,#509,.T.);
#4957=EDGE_CURVE('',#3935,#3933,#510,.T.);
#4958=EDGE_CURVE('',#3936,#3937,#2451,.T.);
#4959=EDGE_CURVE('',#3936,#3934,#511,.T.);
#4960=EDGE_CURVE('',#3937,#3935,#512,.T.);
#4961=EDGE_CURVE('',#3938,#3939,#2452,.T.);
#4962=EDGE_CURVE('',#3938,#3936,#513,.T.);
#4963=EDGE_CURVE('',#3939,#3937,#514,.T.);
#4964=EDGE_CURVE('',#3940,#3941,#2453,.T.);
#4965=EDGE_CURVE('',#3940,#3938,#515,.T.);
#4966=EDGE_CURVE('',#3941,#3939,#516,.T.);
#4967=EDGE_CURVE('',#3942,#3943,#2454,.T.);
#4968=EDGE_CURVE('',#3942,#3940,#517,.T.);
#4969=EDGE_CURVE('',#3943,#3941,#518,.T.);
#4970=EDGE_CURVE('',#3944,#3945,#2455,.T.);
#4971=EDGE_CURVE('',#3944,#3942,#519,.T.);
#4972=EDGE_CURVE('',#3945,#3943,#520,.T.);
#4973=EDGE_CURVE('',#3946,#3947,#2456,.T.);
#4974=EDGE_CURVE('',#3946,#3944,#521,.T.);
#4975=EDGE_CURVE('',#3947,#3945,#522,.T.);
#4976=EDGE_CURVE('',#3948,#3825,#523,.T.);
#4977=EDGE_CURVE('',#3819,#3948,#524,.T.);
#4978=EDGE_CURVE('',#3949,#3695,#525,.T.);
#4979=EDGE_CURVE('',#3949,#3947,#526,.T.);
#4980=EDGE_CURVE('',#3950,#3949,#3281,.T.);
#4981=EDGE_CURVE('',#3950,#3946,#527,.T.);
#4982=EDGE_CURVE('',#3822,#3951,#528,.T.);
#4983=EDGE_CURVE('',#3694,#3950,#529,.T.);
#4984=EDGE_CURVE('',#3951,#3818,#530,.T.);
#4985=EDGE_CURVE('',#3952,#3953,#2457,.T.);
#4986=EDGE_CURVE('',#3952,#3954,#2458,.T.);
#4987=EDGE_CURVE('',#3955,#3954,#2459,.T.);
#4988=EDGE_CURVE('',#3953,#3955,#2460,.T.);
#4989=EDGE_CURVE('',#3953,#3956,#3282,.T.);
#4990=EDGE_CURVE('',#3955,#3957,#2461,.T.);
#4991=EDGE_CURVE('',#3957,#3956,#2462,.T.);
#4992=EDGE_CURVE('',#3954,#3958,#2463,.T.);
#4993=EDGE_CURVE('',#3957,#3958,#2464,.T.);
#4994=EDGE_CURVE('',#3956,#3959,#2465,.T.);
#4995=EDGE_CURVE('',#3958,#3959,#2466,.T.);
#4996=EDGE_CURVE('',#3959,#3952,#3283,.T.);
#4997=EDGE_CURVE('',#3960,#3960,#3284,.T.);
#4998=EDGE_CURVE('',#3960,#3961,#2467,.T.);
#4999=EDGE_CURVE('',#3961,#3961,#3285,.T.);
#5000=EDGE_CURVE('',#3962,#3962,#3286,.T.);
#5001=EDGE_CURVE('',#3951,#3948,#3287,.F.);
#5002=EDGE_CURVE('',#3963,#3963,#3288,.T.);
#5003=EDGE_CURVE('',#3963,#3962,#2468,.T.);
#5004=EDGE_CURVE('',#3964,#3964,#3289,.T.);
#5005=EDGE_CURVE('',#3964,#3965,#2469,.T.);
#5006=EDGE_CURVE('',#3965,#3965,#3290,.T.);
#5007=EDGE_CURVE('',#3966,#3966,#3291,.T.);
#5008=EDGE_CURVE('',#3966,#3967,#2470,.T.);
#5009=EDGE_CURVE('',#3967,#3967,#3292,.T.);
#5010=EDGE_CURVE('',#3968,#3969,#2471,.T.);
#5011=EDGE_CURVE('',#3968,#3969,#3293,.T.);
#5012=EDGE_CURVE('',#3970,#3971,#531,.T.);
#5013=EDGE_CURVE('',#3972,#3970,#3294,.T.);
#5014=EDGE_CURVE('',#3969,#3972,#532,.T.);
#5015=EDGE_CURVE('',#3971,#3968,#533,.T.);
#5016=EDGE_CURVE('',#3971,#3973,#2472,.T.);
#5017=EDGE_CURVE('',#3974,#3973,#534,.T.);
#5018=EDGE_CURVE('',#3973,#3974,#535,.T.);
#5019=EDGE_CURVE('',#3972,#3970,#2473,.T.);
#5020=EDGE_CURVE('',#3975,#3975,#3295,.T.);
#5021=EDGE_CURVE('',#3975,#3976,#2474,.T.);
#5022=EDGE_CURVE('',#3976,#3976,#3296,.T.);
#5023=EDGE_CURVE('',#3977,#3977,#3297,.T.);
#5024=EDGE_CURVE('',#3977,#3978,#2475,.T.);
#5025=EDGE_CURVE('',#3978,#3978,#3298,.T.);
#5026=EDGE_CURVE('',#3979,#3979,#3299,.T.);
#5027=EDGE_CURVE('',#3979,#3980,#2476,.T.);
#5028=EDGE_CURVE('',#3980,#3980,#3300,.T.);
#5029=EDGE_CURVE('',#3981,#3982,#2477,.T.);
#5030=EDGE_CURVE('',#3981,#3982,#3301,.T.);
#5031=EDGE_CURVE('',#3983,#3984,#536,.T.);
#5032=EDGE_CURVE('',#3985,#3983,#3302,.T.);
#5033=EDGE_CURVE('',#3982,#3985,#537,.T.);
#5034=EDGE_CURVE('',#3984,#3981,#538,.T.);
#5035=EDGE_CURVE('',#3984,#3986,#2478,.T.);
#5036=EDGE_CURVE('',#3987,#3986,#539,.T.);
#5037=EDGE_CURVE('',#3986,#3987,#540,.T.);
#5038=EDGE_CURVE('',#3985,#3983,#2479,.T.);
#5039=EDGE_CURVE('',#3988,#3989,#2480,.T.);
#5040=EDGE_CURVE('',#3990,#3988,#2481,.T.);
#5041=EDGE_CURVE('',#3991,#3990,#2482,.T.);
#5042=EDGE_CURVE('',#3992,#3991,#2483,.T.);
#5043=EDGE_CURVE('',#3993,#3992,#2484,.T.);
#5044=EDGE_CURVE('',#3989,#3993,#2485,.T.);
#5045=EDGE_CURVE('',#3994,#3988,#2486,.T.);
#5046=EDGE_CURVE('',#3995,#3994,#2487,.T.);
#5047=EDGE_CURVE('',#3990,#3995,#2488,.T.);
#5048=EDGE_CURVE('',#3996,#3994,#2489,.T.);
#5049=EDGE_CURVE('',#3997,#3996,#2490,.T.);
#5050=EDGE_CURVE('',#3998,#3997,#2491,.T.);
#5051=EDGE_CURVE('',#3999,#3998,#2492,.T.);
#5052=EDGE_CURVE('',#3995,#3999,#2493,.T.);
#5053=EDGE_CURVE('',#4000,#4000,#3303,.T.);
#5054=EDGE_CURVE('',#3989,#3996,#3304,.T.);
#5055=EDGE_CURVE('',#4001,#4001,#3305,.T.);
#5056=EDGE_CURVE('',#3999,#3991,#3306,.T.);
#5057=EDGE_CURVE('',#4000,#4001,#2494,.T.);
#5058=EDGE_CURVE('',#3993,#3997,#3307,.T.);
#5059=EDGE_CURVE('',#3998,#3992,#3308,.T.);
#5060=EDGE_CURVE('',#4002,#4002,#3309,.T.);
#5061=EDGE_CURVE('',#4002,#4003,#2495,.T.);
#5062=EDGE_CURVE('',#4003,#4003,#3310,.T.);
#5063=EDGE_CURVE('',#4004,#4004,#3311,.T.);
#5064=EDGE_CURVE('',#4004,#4005,#2496,.T.);
#5065=EDGE_CURVE('',#4005,#4005,#3312,.T.);
#5066=EDGE_CURVE('',#4006,#4006,#3313,.T.);
#5067=EDGE_CURVE('',#4006,#4007,#2497,.T.);
#5068=EDGE_CURVE('',#4007,#4007,#3314,.T.);
#5069=EDGE_CURVE('',#4008,#4008,#3315,.T.);
#5070=EDGE_CURVE('',#4008,#4009,#2498,.T.);
#5071=EDGE_CURVE('',#4009,#4009,#3316,.T.);
#5072=EDGE_CURVE('',#4010,#4011,#2499,.T.);
#5073=EDGE_CURVE('',#4012,#4010,#2500,.T.);
#5074=EDGE_CURVE('',#4013,#4012,#2501,.T.);
#5075=EDGE_CURVE('',#4014,#4013,#2502,.T.);
#5076=EDGE_CURVE('',#4015,#4014,#2503,.T.);
#5077=EDGE_CURVE('',#4016,#4015,#2504,.T.);
#5078=EDGE_CURVE('',#4017,#4016,#2505,.T.);
#5079=EDGE_CURVE('',#4011,#4017,#2506,.T.);
#5080=EDGE_CURVE('',#4014,#4018,#2507,.T.);
#5081=EDGE_CURVE('',#4018,#4019,#2508,.T.);
#5082=EDGE_CURVE('',#4019,#4015,#2509,.T.);
#5083=EDGE_CURVE('',#4020,#4013,#2510,.T.);
#5084=EDGE_CURVE('',#4020,#4018,#2511,.T.);
#5085=EDGE_CURVE('',#4012,#4021,#2512,.T.);
#5086=EDGE_CURVE('',#4021,#4020,#2513,.T.);
#5087=EDGE_CURVE('',#4022,#4010,#2514,.T.);
#5088=EDGE_CURVE('',#4022,#4021,#2515,.T.);
#5089=EDGE_CURVE('',#4023,#4024,#2516,.T.);
#5090=EDGE_CURVE('',#4019,#4023,#2517,.T.);
#5091=EDGE_CURVE('',#4025,#4022,#2518,.T.);
#5092=EDGE_CURVE('',#4024,#4025,#2519,.T.);
#5093=EDGE_CURVE('',#4016,#4023,#2520,.T.);
#5094=EDGE_CURVE('',#4011,#4025,#2521,.T.);
#5095=EDGE_CURVE('',#4024,#4017,#2522,.T.);
#5096=EDGE_CURVE('',#4026,#4027,#2523,.T.);
#5097=EDGE_CURVE('',#4026,#4028,#2524,.T.);
#5098=EDGE_CURVE('',#4028,#4029,#2525,.T.);
#5099=EDGE_CURVE('',#4027,#4029,#2526,.T.);
#5100=EDGE_CURVE('',#4030,#4026,#2527,.T.);
#5101=EDGE_CURVE('',#4030,#4031,#2528,.T.);
#5102=EDGE_CURVE('',#4031,#4028,#2529,.T.);
#5103=EDGE_CURVE('',#4032,#4030,#2530,.T.);
#5104=EDGE_CURVE('',#4032,#4033,#2531,.T.);
#5105=EDGE_CURVE('',#4033,#4031,#2532,.T.);
#5106=EDGE_CURVE('',#4034,#4032,#2533,.T.);
#5107=EDGE_CURVE('',#4034,#4035,#2534,.T.);
#5108=EDGE_CURVE('',#4035,#4033,#2535,.T.);
#5109=EDGE_CURVE('',#4036,#4034,#2536,.T.);
#5110=EDGE_CURVE('',#4036,#4037,#2537,.T.);
#5111=EDGE_CURVE('',#4037,#4035,#2538,.T.);
#5112=EDGE_CURVE('',#4027,#4036,#2539,.T.);
#5113=EDGE_CURVE('',#4029,#4037,#2540,.T.);
#5114=EDGE_CURVE('',#4038,#4038,#3317,.T.);
#5115=EDGE_CURVE('',#4039,#4039,#3318,.T.);
#5116=EDGE_CURVE('',#4039,#4038,#2541,.T.);
#5117=EDGE_CURVE('',#4040,#4040,#3319,.F.);
#5118=EDGE_CURVE('',#4040,#4039,#2542,.T.);
#5119=EDGE_CURVE('',#4041,#4041,#3320,.T.);
#5120=EDGE_CURVE('',#4041,#4040,#2543,.T.);
#5121=EDGE_CURVE('',#4042,#4042,#3321,.T.);
#5122=EDGE_CURVE('',#4042,#4043,#2544,.T.);
#5123=EDGE_CURVE('',#4043,#4043,#3322,.T.);
#5124=EDGE_CURVE('',#4044,#4044,#3323,.T.);
#5125=EDGE_CURVE('',#4044,#4045,#2545,.T.);
#5126=EDGE_CURVE('',#4045,#4045,#3324,.T.);
#5127=EDGE_CURVE('',#4046,#4046,#3325,.T.);
#5128=EDGE_CURVE('',#4047,#4047,#3326,.T.);
#5129=EDGE_CURVE('',#4047,#4046,#2546,.T.);
#5130=EDGE_CURVE('',#4048,#4048,#3327,.T.);
#5131=EDGE_CURVE('',#4048,#4047,#2547,.T.);
#5132=EDGE_CURVE('',#4049,#4049,#3328,.T.);
#5133=EDGE_CURVE('',#4049,#4048,#2548,.T.);
#5134=EDGE_CURVE('',#4050,#4050,#3329,.T.);
#5135=EDGE_CURVE('',#4051,#4051,#3330,.F.);
#5136=EDGE_CURVE('',#4051,#4050,#2549,.T.);
#5137=EDGE_CURVE('',#4052,#4052,#3331,.F.);
#5138=EDGE_CURVE('',#4052,#4051,#2550,.T.);
#5139=EDGE_CURVE('',#4053,#4053,#3332,.T.);
#5140=EDGE_CURVE('',#4053,#4052,#2551,.T.);
#5141=EDGE_CURVE('',#4054,#4055,#2552,.T.);
#5142=EDGE_CURVE('',#4055,#4056,#2553,.T.);
#5143=EDGE_CURVE('',#4056,#4057,#2554,.T.);
#5144=EDGE_CURVE('',#4054,#4057,#2555,.T.);
#5145=EDGE_CURVE('',#4055,#4058,#2556,.T.);
#5146=EDGE_CURVE('',#4058,#4059,#2557,.T.);
#5147=EDGE_CURVE('',#4059,#4056,#2558,.T.);
#5148=EDGE_CURVE('',#4058,#4060,#2559,.T.);
#5149=EDGE_CURVE('',#4060,#4061,#2560,.T.);
#5150=EDGE_CURVE('',#4061,#4059,#2561,.T.);
#5151=EDGE_CURVE('',#4060,#4062,#2562,.T.);
#5152=EDGE_CURVE('',#4062,#4063,#2563,.T.);
#5153=EDGE_CURVE('',#4063,#4061,#2564,.T.);
#5154=EDGE_CURVE('',#4062,#4064,#2565,.T.);
#5155=EDGE_CURVE('',#4064,#4065,#2566,.T.);
#5156=EDGE_CURVE('',#4065,#4063,#2567,.T.);
#5157=EDGE_CURVE('',#4064,#4054,#2568,.T.);
#5158=EDGE_CURVE('',#4057,#4065,#2569,.T.);
#5159=ORIENTED_EDGE('',*,*,#4066,.F.);
#5160=ORIENTED_EDGE('',*,*,#4067,.T.);
#5161=ORIENTED_EDGE('',*,*,#4068,.F.);
#5162=ORIENTED_EDGE('',*,*,#4067,.F.);
#5163=ORIENTED_EDGE('',*,*,#4069,.F.);
#5164=ORIENTED_EDGE('',*,*,#4070,.T.);
#5165=ORIENTED_EDGE('',*,*,#4071,.F.);
#5166=ORIENTED_EDGE('',*,*,#4070,.F.);
#5167=ORIENTED_EDGE('',*,*,#4072,.F.);
#5168=ORIENTED_EDGE('',*,*,#4073,.T.);
#5169=ORIENTED_EDGE('',*,*,#4074,.F.);
#5170=ORIENTED_EDGE('',*,*,#4073,.F.);
#5171=ORIENTED_EDGE('',*,*,#4075,.F.);
#5172=ORIENTED_EDGE('',*,*,#4076,.T.);
#5173=ORIENTED_EDGE('',*,*,#4077,.F.);
#5174=ORIENTED_EDGE('',*,*,#4076,.F.);
#5175=ORIENTED_EDGE('',*,*,#4078,.F.);
#5176=ORIENTED_EDGE('',*,*,#4079,.T.);
#5177=ORIENTED_EDGE('',*,*,#4080,.F.);
#5178=ORIENTED_EDGE('',*,*,#4079,.F.);
#5179=ORIENTED_EDGE('',*,*,#4081,.F.);
#5180=ORIENTED_EDGE('',*,*,#4082,.T.);
#5181=ORIENTED_EDGE('',*,*,#4083,.F.);
#5182=ORIENTED_EDGE('',*,*,#4082,.F.);
#5183=ORIENTED_EDGE('',*,*,#4084,.F.);
#5184=ORIENTED_EDGE('',*,*,#4085,.T.);
#5185=ORIENTED_EDGE('',*,*,#4086,.F.);
#5186=ORIENTED_EDGE('',*,*,#4085,.F.);
#5187=ORIENTED_EDGE('',*,*,#4087,.T.);
#5188=ORIENTED_EDGE('',*,*,#4088,.T.);
#5189=ORIENTED_EDGE('',*,*,#4089,.F.);
#5190=ORIENTED_EDGE('',*,*,#4090,.F.);
#5191=ORIENTED_EDGE('',*,*,#4091,.T.);
#5192=ORIENTED_EDGE('',*,*,#4090,.T.);
#5193=ORIENTED_EDGE('',*,*,#4092,.F.);
#5194=ORIENTED_EDGE('',*,*,#4093,.F.);
#5195=ORIENTED_EDGE('',*,*,#4094,.T.);
#5196=ORIENTED_EDGE('',*,*,#4093,.T.);
#5197=ORIENTED_EDGE('',*,*,#4095,.F.);
#5198=ORIENTED_EDGE('',*,*,#4096,.F.);
#5199=ORIENTED_EDGE('',*,*,#4097,.T.);
#5200=ORIENTED_EDGE('',*,*,#4096,.T.);
#5201=ORIENTED_EDGE('',*,*,#4098,.F.);
#5202=ORIENTED_EDGE('',*,*,#4088,.F.);
#5203=ORIENTED_EDGE('',*,*,#4098,.T.);
#5204=ORIENTED_EDGE('',*,*,#4095,.T.);
#5205=ORIENTED_EDGE('',*,*,#4092,.T.);
#5206=ORIENTED_EDGE('',*,*,#4089,.T.);
#5207=ORIENTED_EDGE('',*,*,#4086,.T.);
#5208=ORIENTED_EDGE('',*,*,#4083,.T.);
#5209=ORIENTED_EDGE('',*,*,#4080,.T.);
#5210=ORIENTED_EDGE('',*,*,#4077,.T.);
#5211=ORIENTED_EDGE('',*,*,#4074,.T.);
#5212=ORIENTED_EDGE('',*,*,#4071,.T.);
#5213=ORIENTED_EDGE('',*,*,#4068,.T.);
#5214=ORIENTED_EDGE('',*,*,#4097,.F.);
#5215=ORIENTED_EDGE('',*,*,#4087,.F.);
#5216=ORIENTED_EDGE('',*,*,#4091,.F.);
#5217=ORIENTED_EDGE('',*,*,#4094,.F.);
#5218=ORIENTED_EDGE('',*,*,#4084,.T.);
#5219=ORIENTED_EDGE('',*,*,#4081,.T.);
#5220=ORIENTED_EDGE('',*,*,#4078,.T.);
#5221=ORIENTED_EDGE('',*,*,#4075,.T.);
#5222=ORIENTED_EDGE('',*,*,#4072,.T.);
#5223=ORIENTED_EDGE('',*,*,#4069,.T.);
#5224=ORIENTED_EDGE('',*,*,#4066,.T.);
#5225=ORIENTED_EDGE('',*,*,#4099,.F.);
#5226=ORIENTED_EDGE('',*,*,#4100,.T.);
#5227=ORIENTED_EDGE('',*,*,#4101,.T.);
#5228=ORIENTED_EDGE('',*,*,#4100,.F.);
#5229=ORIENTED_EDGE('',*,*,#4101,.F.);
#5230=ORIENTED_EDGE('',*,*,#4102,.F.);
#5231=ORIENTED_EDGE('',*,*,#4103,.T.);
#5232=ORIENTED_EDGE('',*,*,#4104,.T.);
#5233=ORIENTED_EDGE('',*,*,#4103,.F.);
#5234=ORIENTED_EDGE('',*,*,#4104,.F.);
#5235=ORIENTED_EDGE('',*,*,#4105,.F.);
#5236=ORIENTED_EDGE('',*,*,#4106,.T.);
#5237=ORIENTED_EDGE('',*,*,#4107,.T.);
#5238=ORIENTED_EDGE('',*,*,#4106,.F.);
#5239=ORIENTED_EDGE('',*,*,#4107,.F.);
#5240=ORIENTED_EDGE('',*,*,#4108,.T.);
#5241=ORIENTED_EDGE('',*,*,#4109,.T.);
#5242=ORIENTED_EDGE('',*,*,#4110,.F.);
#5243=ORIENTED_EDGE('',*,*,#4111,.F.);
#5244=ORIENTED_EDGE('',*,*,#4112,.T.);
#5245=ORIENTED_EDGE('',*,*,#4111,.T.);
#5246=ORIENTED_EDGE('',*,*,#4113,.F.);
#5247=ORIENTED_EDGE('',*,*,#4114,.F.);
#5248=ORIENTED_EDGE('',*,*,#4115,.T.);
#5249=ORIENTED_EDGE('',*,*,#4114,.T.);
#5250=ORIENTED_EDGE('',*,*,#4116,.F.);
#5251=ORIENTED_EDGE('',*,*,#4117,.F.);
#5252=ORIENTED_EDGE('',*,*,#4099,.T.);
#5253=ORIENTED_EDGE('',*,*,#4102,.T.);
#5254=ORIENTED_EDGE('',*,*,#4105,.T.);
#5255=ORIENTED_EDGE('',*,*,#4118,.T.);
#5256=ORIENTED_EDGE('',*,*,#4117,.T.);
#5257=ORIENTED_EDGE('',*,*,#4119,.F.);
#5258=ORIENTED_EDGE('',*,*,#4109,.F.);
#5259=ORIENTED_EDGE('',*,*,#4119,.T.);
#5260=ORIENTED_EDGE('',*,*,#4116,.T.);
#5261=ORIENTED_EDGE('',*,*,#4113,.T.);
#5262=ORIENTED_EDGE('',*,*,#4110,.T.);
#5263=ORIENTED_EDGE('',*,*,#4118,.F.);
#5264=ORIENTED_EDGE('',*,*,#4108,.F.);
#5265=ORIENTED_EDGE('',*,*,#4112,.F.);
#5266=ORIENTED_EDGE('',*,*,#4115,.F.);
#5267=ORIENTED_EDGE('',*,*,#4120,.F.);
#5268=ORIENTED_EDGE('',*,*,#4121,.T.);
#5269=ORIENTED_EDGE('',*,*,#4122,.F.);
#5270=ORIENTED_EDGE('',*,*,#4121,.F.);
#5271=ORIENTED_EDGE('',*,*,#4120,.T.);
#5272=ORIENTED_EDGE('',*,*,#4123,.F.);
#5273=ORIENTED_EDGE('',*,*,#4124,.T.);
#5274=ORIENTED_EDGE('',*,*,#4125,.F.);
#5275=ORIENTED_EDGE('',*,*,#4124,.F.);
#5276=ORIENTED_EDGE('',*,*,#4123,.T.);
#5277=ORIENTED_EDGE('',*,*,#4126,.F.);
#5278=ORIENTED_EDGE('',*,*,#4127,.T.);
#5279=ORIENTED_EDGE('',*,*,#4128,.T.);
#5280=ORIENTED_EDGE('',*,*,#4127,.F.);
#5281=ORIENTED_EDGE('',*,*,#4128,.F.);
#5282=ORIENTED_EDGE('',*,*,#4129,.F.);
#5283=ORIENTED_EDGE('',*,*,#4130,.T.);
#5284=ORIENTED_EDGE('',*,*,#4131,.T.);
#5285=ORIENTED_EDGE('',*,*,#4130,.F.);
#5286=ORIENTED_EDGE('',*,*,#4131,.F.);
#5287=ORIENTED_EDGE('',*,*,#4132,.T.);
#5288=ORIENTED_EDGE('',*,*,#4133,.T.);
#5289=ORIENTED_EDGE('',*,*,#4134,.F.);
#5290=ORIENTED_EDGE('',*,*,#4135,.F.);
#5291=ORIENTED_EDGE('',*,*,#4136,.T.);
#5292=ORIENTED_EDGE('',*,*,#4135,.T.);
#5293=ORIENTED_EDGE('',*,*,#4137,.F.);
#5294=ORIENTED_EDGE('',*,*,#4138,.F.);
#5295=ORIENTED_EDGE('',*,*,#4122,.T.);
#5296=ORIENTED_EDGE('',*,*,#4125,.T.);
#5297=ORIENTED_EDGE('',*,*,#4139,.T.);
#5298=ORIENTED_EDGE('',*,*,#4138,.T.);
#5299=ORIENTED_EDGE('',*,*,#4140,.F.);
#5300=ORIENTED_EDGE('',*,*,#4141,.F.);
#5301=ORIENTED_EDGE('',*,*,#4142,.T.);
#5302=ORIENTED_EDGE('',*,*,#4141,.T.);
#5303=ORIENTED_EDGE('',*,*,#4143,.F.);
#5304=ORIENTED_EDGE('',*,*,#4133,.F.);
#5305=ORIENTED_EDGE('',*,*,#4143,.T.);
#5306=ORIENTED_EDGE('',*,*,#4140,.T.);
#5307=ORIENTED_EDGE('',*,*,#4137,.T.);
#5308=ORIENTED_EDGE('',*,*,#4134,.T.);
#5309=ORIENTED_EDGE('',*,*,#4142,.F.);
#5310=ORIENTED_EDGE('',*,*,#4132,.F.);
#5311=ORIENTED_EDGE('',*,*,#4136,.F.);
#5312=ORIENTED_EDGE('',*,*,#4139,.F.);
#5313=ORIENTED_EDGE('',*,*,#4126,.T.);
#5314=ORIENTED_EDGE('',*,*,#4129,.T.);
#5315=ORIENTED_EDGE('',*,*,#4144,.F.);
#5316=ORIENTED_EDGE('',*,*,#4145,.T.);
#5317=ORIENTED_EDGE('',*,*,#4146,.F.);
#5318=ORIENTED_EDGE('',*,*,#4145,.F.);
#5319=ORIENTED_EDGE('',*,*,#4147,.F.);
#5320=ORIENTED_EDGE('',*,*,#4148,.T.);
#5321=ORIENTED_EDGE('',*,*,#4149,.F.);
#5322=ORIENTED_EDGE('',*,*,#4148,.F.);
#5323=ORIENTED_EDGE('',*,*,#4150,.F.);
#5324=ORIENTED_EDGE('',*,*,#4151,.T.);
#5325=ORIENTED_EDGE('',*,*,#4152,.F.);
#5326=ORIENTED_EDGE('',*,*,#4151,.F.);
#5327=ORIENTED_EDGE('',*,*,#4153,.F.);
#5328=ORIENTED_EDGE('',*,*,#4154,.T.);
#5329=ORIENTED_EDGE('',*,*,#4155,.F.);
#5330=ORIENTED_EDGE('',*,*,#4154,.F.);
#5331=ORIENTED_EDGE('',*,*,#4153,.T.);
#5332=ORIENTED_EDGE('',*,*,#4156,.F.);
#5333=ORIENTED_EDGE('',*,*,#4157,.F.);
#5334=ORIENTED_EDGE('',*,*,#4158,.T.);
#5335=ORIENTED_EDGE('',*,*,#4156,.T.);
#5336=ORIENTED_EDGE('',*,*,#4158,.F.);
#5337=ORIENTED_EDGE('',*,*,#4159,.F.);
#5338=ORIENTED_EDGE('',*,*,#4160,.T.);
#5339=ORIENTED_EDGE('',*,*,#4161,.T.);
#5340=ORIENTED_EDGE('',*,*,#4160,.F.);
#5341=ORIENTED_EDGE('',*,*,#4161,.F.);
#5342=ORIENTED_EDGE('',*,*,#4162,.F.);
#5343=ORIENTED_EDGE('',*,*,#4163,.T.);
#5344=ORIENTED_EDGE('',*,*,#4164,.T.);
#5345=ORIENTED_EDGE('',*,*,#4163,.F.);
#5346=ORIENTED_EDGE('',*,*,#4164,.F.);
#5347=ORIENTED_EDGE('',*,*,#4165,.T.);
#5348=ORIENTED_EDGE('',*,*,#4166,.T.);
#5349=ORIENTED_EDGE('',*,*,#4167,.F.);
#5350=ORIENTED_EDGE('',*,*,#4168,.F.);
#5351=ORIENTED_EDGE('',*,*,#4169,.T.);
#5352=ORIENTED_EDGE('',*,*,#4168,.T.);
#5353=ORIENTED_EDGE('',*,*,#4170,.F.);
#5354=ORIENTED_EDGE('',*,*,#4171,.F.);
#5355=ORIENTED_EDGE('',*,*,#4146,.T.);
#5356=ORIENTED_EDGE('',*,*,#4149,.T.);
#5357=ORIENTED_EDGE('',*,*,#4152,.T.);
#5358=ORIENTED_EDGE('',*,*,#4155,.T.);
#5359=ORIENTED_EDGE('',*,*,#4172,.T.);
#5360=ORIENTED_EDGE('',*,*,#4171,.T.);
#5361=ORIENTED_EDGE('',*,*,#4173,.F.);
#5362=ORIENTED_EDGE('',*,*,#4174,.F.);
#5363=ORIENTED_EDGE('',*,*,#4175,.T.);
#5364=ORIENTED_EDGE('',*,*,#4174,.T.);
#5365=ORIENTED_EDGE('',*,*,#4176,.F.);
#5366=ORIENTED_EDGE('',*,*,#4166,.F.);
#5367=ORIENTED_EDGE('',*,*,#4144,.T.);
#5368=ORIENTED_EDGE('',*,*,#4147,.T.);
#5369=ORIENTED_EDGE('',*,*,#4150,.T.);
#5370=ORIENTED_EDGE('',*,*,#4157,.T.);
#5371=ORIENTED_EDGE('',*,*,#4176,.T.);
#5372=ORIENTED_EDGE('',*,*,#4173,.T.);
#5373=ORIENTED_EDGE('',*,*,#4170,.T.);
#5374=ORIENTED_EDGE('',*,*,#4167,.T.);
#5375=ORIENTED_EDGE('',*,*,#4175,.F.);
#5376=ORIENTED_EDGE('',*,*,#4165,.F.);
#5377=ORIENTED_EDGE('',*,*,#4169,.F.);
#5378=ORIENTED_EDGE('',*,*,#4172,.F.);
#5379=ORIENTED_EDGE('',*,*,#4159,.T.);
#5380=ORIENTED_EDGE('',*,*,#4162,.T.);
#5381=ORIENTED_EDGE('',*,*,#4177,.F.);
#5382=ORIENTED_EDGE('',*,*,#4178,.T.);
#5383=ORIENTED_EDGE('',*,*,#4179,.F.);
#5384=ORIENTED_EDGE('',*,*,#4178,.F.);
#5385=ORIENTED_EDGE('',*,*,#4180,.F.);
#5386=ORIENTED_EDGE('',*,*,#4181,.T.);
#5387=ORIENTED_EDGE('',*,*,#4182,.F.);
#5388=ORIENTED_EDGE('',*,*,#4181,.F.);
#5389=ORIENTED_EDGE('',*,*,#4183,.F.);
#5390=ORIENTED_EDGE('',*,*,#4184,.T.);
#5391=ORIENTED_EDGE('',*,*,#4185,.F.);
#5392=ORIENTED_EDGE('',*,*,#4184,.F.);
#5393=ORIENTED_EDGE('',*,*,#4186,.F.);
#5394=ORIENTED_EDGE('',*,*,#4187,.F.);
#5395=ORIENTED_EDGE('',*,*,#4188,.F.);
#5396=ORIENTED_EDGE('',*,*,#4189,.F.);
#5397=ORIENTED_EDGE('',*,*,#4187,.T.);
#5398=ORIENTED_EDGE('',*,*,#4190,.F.);
#5399=ORIENTED_EDGE('',*,*,#4177,.T.);
#5400=ORIENTED_EDGE('',*,*,#4180,.T.);
#5401=ORIENTED_EDGE('',*,*,#4183,.T.);
#5402=ORIENTED_EDGE('',*,*,#4191,.T.);
#5403=ORIENTED_EDGE('',*,*,#4188,.T.);
#5404=ORIENTED_EDGE('',*,*,#4190,.T.);
#5405=ORIENTED_EDGE('',*,*,#4186,.T.);
#5406=ORIENTED_EDGE('',*,*,#4192,.F.);
#5407=ORIENTED_EDGE('',*,*,#4191,.F.);
#5408=ORIENTED_EDGE('',*,*,#4193,.T.);
#5409=ORIENTED_EDGE('',*,*,#4194,.T.);
#5410=ORIENTED_EDGE('',*,*,#4193,.F.);
#5411=ORIENTED_EDGE('',*,*,#4194,.F.);
#5412=ORIENTED_EDGE('',*,*,#4195,.F.);
#5413=ORIENTED_EDGE('',*,*,#4196,.F.);
#5414=ORIENTED_EDGE('',*,*,#4197,.T.);
#5415=ORIENTED_EDGE('',*,*,#4195,.T.);
#5416=ORIENTED_EDGE('',*,*,#4197,.F.);
#5417=ORIENTED_EDGE('',*,*,#4189,.T.);
#5418=ORIENTED_EDGE('',*,*,#4192,.T.);
#5419=ORIENTED_EDGE('',*,*,#4179,.T.);
#5420=ORIENTED_EDGE('',*,*,#4182,.T.);
#5421=ORIENTED_EDGE('',*,*,#4185,.T.);
#5422=ORIENTED_EDGE('',*,*,#4196,.T.);
#5423=ORIENTED_EDGE('',*,*,#4198,.F.);
#5424=ORIENTED_EDGE('',*,*,#4199,.F.);
#5425=ORIENTED_EDGE('',*,*,#4200,.F.);
#5426=ORIENTED_EDGE('',*,*,#4201,.F.);
#5427=ORIENTED_EDGE('',*,*,#4200,.T.);
#5428=ORIENTED_EDGE('',*,*,#4202,.T.);
#5429=ORIENTED_EDGE('',*,*,#4203,.T.);
#5430=ORIENTED_EDGE('',*,*,#4204,.F.);
#5431=ORIENTED_EDGE('',*,*,#4205,.T.);
#5432=ORIENTED_EDGE('',*,*,#4206,.T.);
#5433=ORIENTED_EDGE('',*,*,#4199,.T.);
#5434=ORIENTED_EDGE('',*,*,#4207,.F.);
#5435=ORIENTED_EDGE('',*,*,#4208,.T.);
#5436=ORIENTED_EDGE('',*,*,#4202,.F.);
#5437=ORIENTED_EDGE('',*,*,#4203,.F.);
#5438=ORIENTED_EDGE('',*,*,#4208,.F.);
#5439=ORIENTED_EDGE('',*,*,#4209,.F.);
#5440=ORIENTED_EDGE('',*,*,#4210,.F.);
#5441=ORIENTED_EDGE('',*,*,#4198,.T.);
#5442=ORIENTED_EDGE('',*,*,#4211,.F.);
#5443=ORIENTED_EDGE('',*,*,#4209,.T.);
#5444=ORIENTED_EDGE('',*,*,#4207,.T.);
#5445=ORIENTED_EDGE('',*,*,#4212,.T.);
#5446=ORIENTED_EDGE('',*,*,#4213,.T.);
#5447=ORIENTED_EDGE('',*,*,#4214,.F.);
#5448=ORIENTED_EDGE('',*,*,#4215,.T.);
#5449=ORIENTED_EDGE('',*,*,#4213,.F.);
#5450=ORIENTED_EDGE('',*,*,#4215,.F.);
#5451=ORIENTED_EDGE('',*,*,#4214,.T.);
#5452=ORIENTED_EDGE('',*,*,#4216,.F.);
#5453=ORIENTED_EDGE('',*,*,#4217,.F.);
#5454=ORIENTED_EDGE('',*,*,#4218,.T.);
#5455=ORIENTED_EDGE('',*,*,#4212,.F.);
#5456=ORIENTED_EDGE('',*,*,#4218,.F.);
#5457=ORIENTED_EDGE('',*,*,#4217,.T.);
#5458=ORIENTED_EDGE('',*,*,#4219,.F.);
#5459=ORIENTED_EDGE('',*,*,#4206,.F.);
#5460=ORIENTED_EDGE('',*,*,#4220,.T.);
#5461=ORIENTED_EDGE('',*,*,#4216,.T.);
#5462=ORIENTED_EDGE('',*,*,#4220,.F.);
#5463=ORIENTED_EDGE('',*,*,#4205,.F.);
#5464=ORIENTED_EDGE('',*,*,#4221,.T.);
#5465=ORIENTED_EDGE('',*,*,#4219,.T.);
#5466=ORIENTED_EDGE('',*,*,#4221,.F.);
#5467=ORIENTED_EDGE('',*,*,#4201,.T.);
#5468=ORIENTED_EDGE('',*,*,#4204,.T.);
#5469=ORIENTED_EDGE('',*,*,#4210,.T.);
#5470=ORIENTED_EDGE('',*,*,#4211,.T.);
#5471=ORIENTED_EDGE('',*,*,#4222,.T.);
#5472=ORIENTED_EDGE('',*,*,#4223,.T.);
#5473=ORIENTED_EDGE('',*,*,#4224,.T.);
#5474=ORIENTED_EDGE('',*,*,#4225,.F.);
#5475=ORIENTED_EDGE('',*,*,#4226,.T.);
#5476=ORIENTED_EDGE('',*,*,#4227,.T.);
#5477=ORIENTED_EDGE('',*,*,#4228,.T.);
#5478=ORIENTED_EDGE('',*,*,#4223,.F.);
#5479=ORIENTED_EDGE('',*,*,#4229,.T.);
#5480=ORIENTED_EDGE('',*,*,#4230,.T.);
#5481=ORIENTED_EDGE('',*,*,#4231,.T.);
#5482=ORIENTED_EDGE('',*,*,#4227,.F.);
#5483=ORIENTED_EDGE('',*,*,#4232,.T.);
#5484=ORIENTED_EDGE('',*,*,#4233,.T.);
#5485=ORIENTED_EDGE('',*,*,#4234,.T.);
#5486=ORIENTED_EDGE('',*,*,#4230,.F.);
#5487=ORIENTED_EDGE('',*,*,#4235,.T.);
#5488=ORIENTED_EDGE('',*,*,#4236,.T.);
#5489=ORIENTED_EDGE('',*,*,#4237,.T.);
#5490=ORIENTED_EDGE('',*,*,#4233,.F.);
#5491=ORIENTED_EDGE('',*,*,#4238,.T.);
#5492=ORIENTED_EDGE('',*,*,#4225,.T.);
#5493=ORIENTED_EDGE('',*,*,#4239,.T.);
#5494=ORIENTED_EDGE('',*,*,#4236,.F.);
#5495=ORIENTED_EDGE('',*,*,#4238,.F.);
#5496=ORIENTED_EDGE('',*,*,#4235,.F.);
#5497=ORIENTED_EDGE('',*,*,#4232,.F.);
#5498=ORIENTED_EDGE('',*,*,#4229,.F.);
#5499=ORIENTED_EDGE('',*,*,#4226,.F.);
#5500=ORIENTED_EDGE('',*,*,#4222,.F.);
#5501=ORIENTED_EDGE('',*,*,#4239,.F.);
#5502=ORIENTED_EDGE('',*,*,#4224,.F.);
#5503=ORIENTED_EDGE('',*,*,#4228,.F.);
#5504=ORIENTED_EDGE('',*,*,#4231,.F.);
#5505=ORIENTED_EDGE('',*,*,#4234,.F.);
#5506=ORIENTED_EDGE('',*,*,#4237,.F.);
#5507=ORIENTED_EDGE('',*,*,#4240,.F.);
#5508=ORIENTED_EDGE('',*,*,#4241,.F.);
#5509=ORIENTED_EDGE('',*,*,#4242,.F.);
#5510=ORIENTED_EDGE('',*,*,#4243,.T.);
#5511=ORIENTED_EDGE('',*,*,#4241,.T.);
#5512=ORIENTED_EDGE('',*,*,#4243,.F.);
#5513=ORIENTED_EDGE('',*,*,#4244,.F.);
#5514=ORIENTED_EDGE('',*,*,#4245,.T.);
#5515=ORIENTED_EDGE('',*,*,#4242,.T.);
#5516=ORIENTED_EDGE('',*,*,#4245,.F.);
#5517=ORIENTED_EDGE('',*,*,#4246,.F.);
#5518=ORIENTED_EDGE('',*,*,#4247,.T.);
#5519=ORIENTED_EDGE('',*,*,#4244,.T.);
#5520=ORIENTED_EDGE('',*,*,#4247,.F.);
#5521=ORIENTED_EDGE('',*,*,#4246,.T.);
#5522=ORIENTED_EDGE('',*,*,#4248,.F.);
#5523=ORIENTED_EDGE('',*,*,#4249,.F.);
#5524=ORIENTED_EDGE('',*,*,#4250,.T.);
#5525=ORIENTED_EDGE('',*,*,#4248,.T.);
#5526=ORIENTED_EDGE('',*,*,#4250,.F.);
#5527=ORIENTED_EDGE('',*,*,#4240,.T.);
#5528=ORIENTED_EDGE('',*,*,#4251,.T.);
#5529=ORIENTED_EDGE('',*,*,#4249,.T.);
#5530=ORIENTED_EDGE('',*,*,#4251,.F.);
#5531=ORIENTED_EDGE('',*,*,#4252,.F.);
#5532=ORIENTED_EDGE('',*,*,#4253,.F.);
#5533=ORIENTED_EDGE('',*,*,#4254,.T.);
#5534=ORIENTED_EDGE('',*,*,#4255,.F.);
#5535=ORIENTED_EDGE('',*,*,#4256,.F.);
#5536=ORIENTED_EDGE('',*,*,#4254,.F.);
#5537=ORIENTED_EDGE('',*,*,#4255,.T.);
#5538=ORIENTED_EDGE('',*,*,#4256,.T.);
#5539=ORIENTED_EDGE('',*,*,#4257,.T.);
#5540=ORIENTED_EDGE('',*,*,#4258,.T.);
#5541=ORIENTED_EDGE('',*,*,#4257,.F.);
#5542=ORIENTED_EDGE('',*,*,#4259,.T.);
#5543=ORIENTED_EDGE('',*,*,#4260,.T.);
#5544=ORIENTED_EDGE('',*,*,#4261,.F.);
#5545=ORIENTED_EDGE('',*,*,#4260,.F.);
#5546=ORIENTED_EDGE('',*,*,#4261,.T.);
#5547=ORIENTED_EDGE('',*,*,#4262,.T.);
#5548=ORIENTED_EDGE('',*,*,#4263,.F.);
#5549=ORIENTED_EDGE('',*,*,#4262,.F.);
#5550=ORIENTED_EDGE('',*,*,#4258,.F.);
#5551=ORIENTED_EDGE('',*,*,#4263,.T.);
#5552=ORIENTED_EDGE('',*,*,#4264,.F.);
#5553=ORIENTED_EDGE('',*,*,#4265,.T.);
#5554=ORIENTED_EDGE('',*,*,#4252,.T.);
#5555=ORIENTED_EDGE('',*,*,#4253,.T.);
#5556=ORIENTED_EDGE('',*,*,#4265,.F.);
#5557=ORIENTED_EDGE('',*,*,#4264,.T.);
#5558=ORIENTED_EDGE('',*,*,#4266,.F.);
#5559=ORIENTED_EDGE('',*,*,#4266,.T.);
#5560=ORIENTED_EDGE('',*,*,#4267,.T.);
#5561=ORIENTED_EDGE('',*,*,#4259,.F.);
#5562=ORIENTED_EDGE('',*,*,#4267,.F.);
#5563=ORIENTED_EDGE('',*,*,#4268,.F.);
#5564=ORIENTED_EDGE('',*,*,#4269,.F.);
#5565=ORIENTED_EDGE('',*,*,#4270,.T.);
#5566=ORIENTED_EDGE('',*,*,#4271,.F.);
#5567=ORIENTED_EDGE('',*,*,#4272,.F.);
#5568=ORIENTED_EDGE('',*,*,#4270,.F.);
#5569=ORIENTED_EDGE('',*,*,#4273,.T.);
#5570=ORIENTED_EDGE('',*,*,#4274,.T.);
#5571=ORIENTED_EDGE('',*,*,#4271,.T.);
#5572=ORIENTED_EDGE('',*,*,#4272,.T.);
#5573=ORIENTED_EDGE('',*,*,#4274,.F.);
#5574=ORIENTED_EDGE('',*,*,#4275,.F.);
#5575=ORIENTED_EDGE('',*,*,#4276,.T.);
#5576=ORIENTED_EDGE('',*,*,#4277,.F.);
#5577=ORIENTED_EDGE('',*,*,#4278,.T.);
#5578=ORIENTED_EDGE('',*,*,#4275,.T.);
#5579=ORIENTED_EDGE('',*,*,#4278,.F.);
#5580=ORIENTED_EDGE('',*,*,#4279,.F.);
#5581=ORIENTED_EDGE('',*,*,#4280,.T.);
#5582=ORIENTED_EDGE('',*,*,#4277,.T.);
#5583=ORIENTED_EDGE('',*,*,#4280,.F.);
#5584=ORIENTED_EDGE('',*,*,#4281,.F.);
#5585=ORIENTED_EDGE('',*,*,#4282,.T.);
#5586=ORIENTED_EDGE('',*,*,#4279,.T.);
#5587=ORIENTED_EDGE('',*,*,#4282,.F.);
#5588=ORIENTED_EDGE('',*,*,#4281,.T.);
#5589=ORIENTED_EDGE('',*,*,#4273,.F.);
#5590=ORIENTED_EDGE('',*,*,#4268,.T.);
#5591=ORIENTED_EDGE('',*,*,#4269,.T.);
#5592=ORIENTED_EDGE('',*,*,#4283,.T.);
#5593=ORIENTED_EDGE('',*,*,#4276,.F.);
#5594=ORIENTED_EDGE('',*,*,#4283,.F.);
#5595=ORIENTED_EDGE('',*,*,#4284,.T.);
#5596=ORIENTED_EDGE('',*,*,#4284,.F.);
#5597=ORIENTED_EDGE('',*,*,#4285,.T.);
#5598=ORIENTED_EDGE('',*,*,#4285,.F.);
#5599=ORIENTED_EDGE('',*,*,#4286,.T.);
#5600=ORIENTED_EDGE('',*,*,#4286,.F.);
#5601=ORIENTED_EDGE('',*,*,#4287,.T.);
#5602=ORIENTED_EDGE('',*,*,#4287,.F.);
#5603=ORIENTED_EDGE('',*,*,#4288,.T.);
#5604=ORIENTED_EDGE('',*,*,#4288,.F.);
#5605=ORIENTED_EDGE('',*,*,#4289,.T.);
#5606=ORIENTED_EDGE('',*,*,#4289,.F.);
#5607=ORIENTED_EDGE('',*,*,#4290,.T.);
#5608=ORIENTED_EDGE('',*,*,#4290,.F.);
#5609=ORIENTED_EDGE('',*,*,#4291,.T.);
#5610=ORIENTED_EDGE('',*,*,#4291,.F.);
#5611=ORIENTED_EDGE('',*,*,#4292,.F.);
#5612=ORIENTED_EDGE('',*,*,#4293,.F.);
#5613=ORIENTED_EDGE('',*,*,#4294,.F.);
#5614=ORIENTED_EDGE('',*,*,#4295,.F.);
#5615=ORIENTED_EDGE('',*,*,#4294,.T.);
#5616=ORIENTED_EDGE('',*,*,#4296,.F.);
#5617=ORIENTED_EDGE('',*,*,#4297,.T.);
#5618=ORIENTED_EDGE('',*,*,#4298,.F.);
#5619=ORIENTED_EDGE('',*,*,#4299,.T.);
#5620=ORIENTED_EDGE('',*,*,#4300,.F.);
#5621=ORIENTED_EDGE('',*,*,#4301,.T.);
#5622=ORIENTED_EDGE('',*,*,#4302,.T.);
#5623=ORIENTED_EDGE('',*,*,#4303,.F.);
#5624=ORIENTED_EDGE('',*,*,#4302,.F.);
#5625=ORIENTED_EDGE('',*,*,#4304,.T.);
#5626=ORIENTED_EDGE('',*,*,#4305,.F.);
#5627=ORIENTED_EDGE('',*,*,#4306,.T.);
#5628=ORIENTED_EDGE('',*,*,#4307,.F.);
#5629=ORIENTED_EDGE('',*,*,#4308,.T.);
#5630=ORIENTED_EDGE('',*,*,#4309,.F.);
#5631=ORIENTED_EDGE('',*,*,#4310,.T.);
#5632=ORIENTED_EDGE('',*,*,#4311,.F.);
#5633=ORIENTED_EDGE('',*,*,#4312,.T.);
#5634=ORIENTED_EDGE('',*,*,#4313,.F.);
#5635=ORIENTED_EDGE('',*,*,#4293,.T.);
#5636=ORIENTED_EDGE('',*,*,#4314,.T.);
#5637=ORIENTED_EDGE('',*,*,#4315,.T.);
#5638=ORIENTED_EDGE('',*,*,#4296,.T.);
#5639=ORIENTED_EDGE('',*,*,#4316,.F.);
#5640=ORIENTED_EDGE('',*,*,#4317,.F.);
#5641=ORIENTED_EDGE('',*,*,#4297,.F.);
#5642=ORIENTED_EDGE('',*,*,#4315,.F.);
#5643=ORIENTED_EDGE('',*,*,#4317,.T.);
#5644=ORIENTED_EDGE('',*,*,#4318,.T.);
#5645=ORIENTED_EDGE('',*,*,#4319,.T.);
#5646=ORIENTED_EDGE('',*,*,#4298,.T.);
#5647=ORIENTED_EDGE('',*,*,#4320,.F.);
#5648=ORIENTED_EDGE('',*,*,#4321,.F.);
#5649=ORIENTED_EDGE('',*,*,#4299,.F.);
#5650=ORIENTED_EDGE('',*,*,#4319,.F.);
#5651=ORIENTED_EDGE('',*,*,#4321,.T.);
#5652=ORIENTED_EDGE('',*,*,#4322,.T.);
#5653=ORIENTED_EDGE('',*,*,#4323,.T.);
#5654=ORIENTED_EDGE('',*,*,#4300,.T.);
#5655=ORIENTED_EDGE('',*,*,#4324,.F.);
#5656=ORIENTED_EDGE('',*,*,#4325,.F.);
#5657=ORIENTED_EDGE('',*,*,#4304,.F.);
#5658=ORIENTED_EDGE('',*,*,#4301,.F.);
#5659=ORIENTED_EDGE('',*,*,#4323,.F.);
#5660=ORIENTED_EDGE('',*,*,#4326,.F.);
#5661=ORIENTED_EDGE('',*,*,#4325,.T.);
#5662=ORIENTED_EDGE('',*,*,#4327,.T.);
#5663=ORIENTED_EDGE('',*,*,#4328,.T.);
#5664=ORIENTED_EDGE('',*,*,#4305,.T.);
#5665=ORIENTED_EDGE('',*,*,#4329,.F.);
#5666=ORIENTED_EDGE('',*,*,#4330,.F.);
#5667=ORIENTED_EDGE('',*,*,#4306,.F.);
#5668=ORIENTED_EDGE('',*,*,#4328,.F.);
#5669=ORIENTED_EDGE('',*,*,#4330,.T.);
#5670=ORIENTED_EDGE('',*,*,#4331,.T.);
#5671=ORIENTED_EDGE('',*,*,#4332,.T.);
#5672=ORIENTED_EDGE('',*,*,#4307,.T.);
#5673=ORIENTED_EDGE('',*,*,#4333,.F.);
#5674=ORIENTED_EDGE('',*,*,#4334,.F.);
#5675=ORIENTED_EDGE('',*,*,#4308,.F.);
#5676=ORIENTED_EDGE('',*,*,#4332,.F.);
#5677=ORIENTED_EDGE('',*,*,#4334,.T.);
#5678=ORIENTED_EDGE('',*,*,#4335,.T.);
#5679=ORIENTED_EDGE('',*,*,#4336,.T.);
#5680=ORIENTED_EDGE('',*,*,#4309,.T.);
#5681=ORIENTED_EDGE('',*,*,#4310,.F.);
#5682=ORIENTED_EDGE('',*,*,#4336,.F.);
#5683=ORIENTED_EDGE('',*,*,#4337,.F.);
#5684=ORIENTED_EDGE('',*,*,#4338,.F.);
#5685=ORIENTED_EDGE('',*,*,#4339,.F.);
#5686=ORIENTED_EDGE('',*,*,#4340,.T.);
#5687=ORIENTED_EDGE('',*,*,#4326,.T.);
#5688=ORIENTED_EDGE('',*,*,#4322,.F.);
#5689=ORIENTED_EDGE('',*,*,#4320,.T.);
#5690=ORIENTED_EDGE('',*,*,#4318,.F.);
#5691=ORIENTED_EDGE('',*,*,#4316,.T.);
#5692=ORIENTED_EDGE('',*,*,#4314,.F.);
#5693=ORIENTED_EDGE('',*,*,#4292,.T.);
#5694=ORIENTED_EDGE('',*,*,#4341,.F.);
#5695=ORIENTED_EDGE('',*,*,#4342,.T.);
#5696=ORIENTED_EDGE('',*,*,#4343,.F.);
#5697=ORIENTED_EDGE('',*,*,#4337,.T.);
#5698=ORIENTED_EDGE('',*,*,#4335,.F.);
#5699=ORIENTED_EDGE('',*,*,#4333,.T.);
#5700=ORIENTED_EDGE('',*,*,#4331,.F.);
#5701=ORIENTED_EDGE('',*,*,#4329,.T.);
#5702=ORIENTED_EDGE('',*,*,#4327,.F.);
#5703=ORIENTED_EDGE('',*,*,#4324,.T.);
#5704=ORIENTED_EDGE('',*,*,#4340,.F.);
#5705=ORIENTED_EDGE('',*,*,#4295,.T.);
#5706=ORIENTED_EDGE('',*,*,#4313,.T.);
#5707=ORIENTED_EDGE('',*,*,#4344,.T.);
#5708=ORIENTED_EDGE('',*,*,#4341,.T.);
#5709=ORIENTED_EDGE('',*,*,#4312,.F.);
#5710=ORIENTED_EDGE('',*,*,#4345,.F.);
#5711=ORIENTED_EDGE('',*,*,#4342,.F.);
#5712=ORIENTED_EDGE('',*,*,#4344,.F.);
#5713=ORIENTED_EDGE('',*,*,#4303,.T.);
#5714=ORIENTED_EDGE('',*,*,#4339,.T.);
#5715=ORIENTED_EDGE('',*,*,#4338,.T.);
#5716=ORIENTED_EDGE('',*,*,#4343,.T.);
#5717=ORIENTED_EDGE('',*,*,#4345,.T.);
#5718=ORIENTED_EDGE('',*,*,#4311,.T.);
#5719=ORIENTED_EDGE('',*,*,#4346,.F.);
#5720=ORIENTED_EDGE('',*,*,#4347,.T.);
#5721=ORIENTED_EDGE('',*,*,#4348,.F.);
#5722=ORIENTED_EDGE('',*,*,#4349,.T.);
#5723=ORIENTED_EDGE('',*,*,#4346,.T.);
#5724=ORIENTED_EDGE('',*,*,#4349,.F.);
#5725=ORIENTED_EDGE('',*,*,#4348,.T.);
#5726=ORIENTED_EDGE('',*,*,#4350,.F.);
#5727=ORIENTED_EDGE('',*,*,#4350,.T.);
#5728=ORIENTED_EDGE('',*,*,#4351,.T.);
#5729=ORIENTED_EDGE('',*,*,#4347,.F.);
#5730=ORIENTED_EDGE('',*,*,#4351,.F.);
#5731=ORIENTED_EDGE('',*,*,#4352,.F.);
#5732=ORIENTED_EDGE('',*,*,#4353,.T.);
#5733=ORIENTED_EDGE('',*,*,#4354,.F.);
#5734=ORIENTED_EDGE('',*,*,#4355,.T.);
#5735=ORIENTED_EDGE('',*,*,#4352,.T.);
#5736=ORIENTED_EDGE('',*,*,#4355,.F.);
#5737=ORIENTED_EDGE('',*,*,#4354,.T.);
#5738=ORIENTED_EDGE('',*,*,#4356,.F.);
#5739=ORIENTED_EDGE('',*,*,#4356,.T.);
#5740=ORIENTED_EDGE('',*,*,#4357,.T.);
#5741=ORIENTED_EDGE('',*,*,#4353,.F.);
#5742=ORIENTED_EDGE('',*,*,#4357,.F.);
#5743=ORIENTED_EDGE('',*,*,#4358,.F.);
#5744=ORIENTED_EDGE('',*,*,#4359,.T.);
#5745=ORIENTED_EDGE('',*,*,#4360,.F.);
#5746=ORIENTED_EDGE('',*,*,#4359,.F.);
#5747=ORIENTED_EDGE('',*,*,#4358,.T.);
#5748=ORIENTED_EDGE('',*,*,#4361,.F.);
#5749=ORIENTED_EDGE('',*,*,#4362,.T.);
#5750=ORIENTED_EDGE('',*,*,#4363,.F.);
#5751=ORIENTED_EDGE('',*,*,#4362,.F.);
#5752=ORIENTED_EDGE('',*,*,#4361,.T.);
#5753=ORIENTED_EDGE('',*,*,#4364,.F.);
#5754=ORIENTED_EDGE('',*,*,#4365,.T.);
#5755=ORIENTED_EDGE('',*,*,#4366,.F.);
#5756=ORIENTED_EDGE('',*,*,#4365,.F.);
#5757=ORIENTED_EDGE('',*,*,#4364,.T.);
#5758=ORIENTED_EDGE('',*,*,#4367,.F.);
#5759=ORIENTED_EDGE('',*,*,#4368,.T.);
#5760=ORIENTED_EDGE('',*,*,#4369,.T.);
#5761=ORIENTED_EDGE('',*,*,#4368,.F.);
#5762=ORIENTED_EDGE('',*,*,#4369,.F.);
#5763=ORIENTED_EDGE('',*,*,#4370,.F.);
#5764=ORIENTED_EDGE('',*,*,#4371,.T.);
#5765=ORIENTED_EDGE('',*,*,#4372,.T.);
#5766=ORIENTED_EDGE('',*,*,#4371,.F.);
#5767=ORIENTED_EDGE('',*,*,#4372,.F.);
#5768=ORIENTED_EDGE('',*,*,#4373,.F.);
#5769=ORIENTED_EDGE('',*,*,#4374,.T.);
#5770=ORIENTED_EDGE('',*,*,#4375,.F.);
#5771=ORIENTED_EDGE('',*,*,#4374,.F.);
#5772=ORIENTED_EDGE('',*,*,#4373,.T.);
#5773=ORIENTED_EDGE('',*,*,#4376,.F.);
#5774=ORIENTED_EDGE('',*,*,#4377,.F.);
#5775=ORIENTED_EDGE('',*,*,#4378,.T.);
#5776=ORIENTED_EDGE('',*,*,#4376,.T.);
#5777=ORIENTED_EDGE('',*,*,#4378,.F.);
#5778=ORIENTED_EDGE('',*,*,#4379,.F.);
#5779=ORIENTED_EDGE('',*,*,#4380,.T.);
#5780=ORIENTED_EDGE('',*,*,#4381,.F.);
#5781=ORIENTED_EDGE('',*,*,#4380,.F.);
#5782=ORIENTED_EDGE('',*,*,#4379,.T.);
#5783=ORIENTED_EDGE('',*,*,#4382,.F.);
#5784=ORIENTED_EDGE('',*,*,#4383,.F.);
#5785=ORIENTED_EDGE('',*,*,#4384,.T.);
#5786=ORIENTED_EDGE('',*,*,#4382,.T.);
#5787=ORIENTED_EDGE('',*,*,#4384,.F.);
#5788=ORIENTED_EDGE('',*,*,#4385,.F.);
#5789=ORIENTED_EDGE('',*,*,#4386,.T.);
#5790=ORIENTED_EDGE('',*,*,#4387,.F.);
#5791=ORIENTED_EDGE('',*,*,#4386,.F.);
#5792=ORIENTED_EDGE('',*,*,#4388,.F.);
#5793=ORIENTED_EDGE('',*,*,#4389,.F.);
#5794=ORIENTED_EDGE('',*,*,#4390,.F.);
#5795=ORIENTED_EDGE('',*,*,#4391,.F.);
#5796=ORIENTED_EDGE('',*,*,#4377,.T.);
#5797=ORIENTED_EDGE('',*,*,#4383,.T.);
#5798=ORIENTED_EDGE('',*,*,#4392,.F.);
#5799=ORIENTED_EDGE('',*,*,#4393,.F.);
#5800=ORIENTED_EDGE('',*,*,#4394,.F.);
#5801=ORIENTED_EDGE('',*,*,#4389,.T.);
#5802=ORIENTED_EDGE('',*,*,#4395,.F.);
#5803=ORIENTED_EDGE('',*,*,#4396,.F.);
#5804=ORIENTED_EDGE('',*,*,#4397,.F.);
#5805=ORIENTED_EDGE('',*,*,#4393,.T.);
#5806=ORIENTED_EDGE('',*,*,#4395,.T.);
#5807=ORIENTED_EDGE('',*,*,#4392,.T.);
#5808=ORIENTED_EDGE('',*,*,#4388,.T.);
#5809=ORIENTED_EDGE('',*,*,#4398,.T.);
#5810=ORIENTED_EDGE('',*,*,#4399,.T.);
#5811=ORIENTED_EDGE('',*,*,#4400,.F.);
#5812=ORIENTED_EDGE('',*,*,#4401,.F.);
#5813=ORIENTED_EDGE('',*,*,#4402,.T.);
#5814=ORIENTED_EDGE('',*,*,#4360,.T.);
#5815=ORIENTED_EDGE('',*,*,#4363,.T.);
#5816=ORIENTED_EDGE('',*,*,#4366,.T.);
#5817=ORIENTED_EDGE('',*,*,#4387,.T.);
#5818=ORIENTED_EDGE('',*,*,#4391,.T.);
#5819=ORIENTED_EDGE('',*,*,#4403,.F.);
#5820=ORIENTED_EDGE('',*,*,#4404,.F.);
#5821=ORIENTED_EDGE('',*,*,#4398,.F.);
#5822=ORIENTED_EDGE('',*,*,#4404,.T.);
#5823=ORIENTED_EDGE('',*,*,#4405,.T.);
#5824=ORIENTED_EDGE('',*,*,#4406,.F.);
#5825=ORIENTED_EDGE('',*,*,#4399,.F.);
#5826=ORIENTED_EDGE('',*,*,#4375,.T.);
#5827=ORIENTED_EDGE('',*,*,#4381,.T.);
#5828=ORIENTED_EDGE('',*,*,#4407,.T.);
#5829=ORIENTED_EDGE('',*,*,#4401,.T.);
#5830=ORIENTED_EDGE('',*,*,#4408,.F.);
#5831=ORIENTED_EDGE('',*,*,#4409,.F.);
#5832=ORIENTED_EDGE('',*,*,#4397,.T.);
#5833=ORIENTED_EDGE('',*,*,#4410,.T.);
#5834=ORIENTED_EDGE('',*,*,#4409,.T.);
#5835=ORIENTED_EDGE('',*,*,#4411,.F.);
#5836=ORIENTED_EDGE('',*,*,#4405,.F.);
#5837=ORIENTED_EDGE('',*,*,#4403,.T.);
#5838=ORIENTED_EDGE('',*,*,#4390,.T.);
#5839=ORIENTED_EDGE('',*,*,#4394,.T.);
#5840=ORIENTED_EDGE('',*,*,#4367,.T.);
#5841=ORIENTED_EDGE('',*,*,#4370,.T.);
#5842=ORIENTED_EDGE('',*,*,#4385,.T.);
#5843=ORIENTED_EDGE('',*,*,#4411,.T.);
#5844=ORIENTED_EDGE('',*,*,#4408,.T.);
#5845=ORIENTED_EDGE('',*,*,#4400,.T.);
#5846=ORIENTED_EDGE('',*,*,#4406,.T.);
#5847=ORIENTED_EDGE('',*,*,#4396,.T.);
#5848=ORIENTED_EDGE('',*,*,#4402,.F.);
#5849=ORIENTED_EDGE('',*,*,#4407,.F.);
#5850=ORIENTED_EDGE('',*,*,#4410,.F.);
#5851=ORIENTED_EDGE('',*,*,#4412,.T.);
#5852=ORIENTED_EDGE('',*,*,#4413,.T.);
#5853=ORIENTED_EDGE('',*,*,#4414,.F.);
#5854=ORIENTED_EDGE('',*,*,#4415,.F.);
#5855=ORIENTED_EDGE('',*,*,#4416,.T.);
#5856=ORIENTED_EDGE('',*,*,#4415,.T.);
#5857=ORIENTED_EDGE('',*,*,#4417,.F.);
#5858=ORIENTED_EDGE('',*,*,#4418,.F.);
#5859=ORIENTED_EDGE('',*,*,#4419,.T.);
#5860=ORIENTED_EDGE('',*,*,#4418,.T.);
#5861=ORIENTED_EDGE('',*,*,#4420,.F.);
#5862=ORIENTED_EDGE('',*,*,#4421,.F.);
#5863=ORIENTED_EDGE('',*,*,#4422,.T.);
#5864=ORIENTED_EDGE('',*,*,#4421,.T.);
#5865=ORIENTED_EDGE('',*,*,#4423,.F.);
#5866=ORIENTED_EDGE('',*,*,#4413,.F.);
#5867=ORIENTED_EDGE('',*,*,#4423,.T.);
#5868=ORIENTED_EDGE('',*,*,#4420,.T.);
#5869=ORIENTED_EDGE('',*,*,#4417,.T.);
#5870=ORIENTED_EDGE('',*,*,#4414,.T.);
#5871=ORIENTED_EDGE('',*,*,#4422,.F.);
#5872=ORIENTED_EDGE('',*,*,#4412,.F.);
#5873=ORIENTED_EDGE('',*,*,#4416,.F.);
#5874=ORIENTED_EDGE('',*,*,#4419,.F.);
#5875=ORIENTED_EDGE('',*,*,#4424,.F.);
#5876=ORIENTED_EDGE('',*,*,#4425,.F.);
#5877=ORIENTED_EDGE('',*,*,#4426,.F.);
#5878=ORIENTED_EDGE('',*,*,#4427,.F.);
#5879=ORIENTED_EDGE('',*,*,#4426,.T.);
#5880=ORIENTED_EDGE('',*,*,#4428,.T.);
#5881=ORIENTED_EDGE('',*,*,#4429,.T.);
#5882=ORIENTED_EDGE('',*,*,#4430,.F.);
#5883=ORIENTED_EDGE('',*,*,#4431,.T.);
#5884=ORIENTED_EDGE('',*,*,#4432,.T.);
#5885=ORIENTED_EDGE('',*,*,#4425,.T.);
#5886=ORIENTED_EDGE('',*,*,#4433,.F.);
#5887=ORIENTED_EDGE('',*,*,#4434,.T.);
#5888=ORIENTED_EDGE('',*,*,#4428,.F.);
#5889=ORIENTED_EDGE('',*,*,#4429,.F.);
#5890=ORIENTED_EDGE('',*,*,#4434,.F.);
#5891=ORIENTED_EDGE('',*,*,#4435,.F.);
#5892=ORIENTED_EDGE('',*,*,#4436,.F.);
#5893=ORIENTED_EDGE('',*,*,#4424,.T.);
#5894=ORIENTED_EDGE('',*,*,#4437,.F.);
#5895=ORIENTED_EDGE('',*,*,#4435,.T.);
#5896=ORIENTED_EDGE('',*,*,#4433,.T.);
#5897=ORIENTED_EDGE('',*,*,#4438,.T.);
#5898=ORIENTED_EDGE('',*,*,#4439,.T.);
#5899=ORIENTED_EDGE('',*,*,#4432,.F.);
#5900=ORIENTED_EDGE('',*,*,#4440,.T.);
#5901=ORIENTED_EDGE('',*,*,#4441,.T.);
#5902=ORIENTED_EDGE('',*,*,#4440,.F.);
#5903=ORIENTED_EDGE('',*,*,#4441,.F.);
#5904=ORIENTED_EDGE('',*,*,#4442,.F.);
#5905=ORIENTED_EDGE('',*,*,#4431,.F.);
#5906=ORIENTED_EDGE('',*,*,#4443,.T.);
#5907=ORIENTED_EDGE('',*,*,#4444,.T.);
#5908=ORIENTED_EDGE('',*,*,#4443,.F.);
#5909=ORIENTED_EDGE('',*,*,#4444,.F.);
#5910=ORIENTED_EDGE('',*,*,#4445,.F.);
#5911=ORIENTED_EDGE('',*,*,#4442,.T.);
#5912=ORIENTED_EDGE('',*,*,#4446,.T.);
#5913=ORIENTED_EDGE('',*,*,#4439,.F.);
#5914=ORIENTED_EDGE('',*,*,#4446,.F.);
#5915=ORIENTED_EDGE('',*,*,#4445,.T.);
#5916=ORIENTED_EDGE('',*,*,#4447,.T.);
#5917=ORIENTED_EDGE('',*,*,#4438,.F.);
#5918=ORIENTED_EDGE('',*,*,#4447,.F.);
#5919=ORIENTED_EDGE('',*,*,#4427,.T.);
#5920=ORIENTED_EDGE('',*,*,#4430,.T.);
#5921=ORIENTED_EDGE('',*,*,#4436,.T.);
#5922=ORIENTED_EDGE('',*,*,#4437,.T.);
#5923=ORIENTED_EDGE('',*,*,#4448,.T.);
#5924=ORIENTED_EDGE('',*,*,#4449,.T.);
#5925=ORIENTED_EDGE('',*,*,#4450,.T.);
#5926=ORIENTED_EDGE('',*,*,#4451,.T.);
#5927=ORIENTED_EDGE('',*,*,#4452,.T.);
#5928=ORIENTED_EDGE('',*,*,#4453,.T.);
#5929=ORIENTED_EDGE('',*,*,#4448,.F.);
#5930=ORIENTED_EDGE('',*,*,#4454,.T.);
#5931=ORIENTED_EDGE('',*,*,#4455,.T.);
#5932=ORIENTED_EDGE('',*,*,#4456,.T.);
#5933=ORIENTED_EDGE('',*,*,#4452,.F.);
#5934=ORIENTED_EDGE('',*,*,#4457,.T.);
#5935=ORIENTED_EDGE('',*,*,#4458,.T.);
#5936=ORIENTED_EDGE('',*,*,#4459,.T.);
#5937=ORIENTED_EDGE('',*,*,#4455,.F.);
#5938=ORIENTED_EDGE('',*,*,#4460,.T.);
#5939=ORIENTED_EDGE('',*,*,#4461,.T.);
#5940=ORIENTED_EDGE('',*,*,#4462,.T.);
#5941=ORIENTED_EDGE('',*,*,#4458,.F.);
#5942=ORIENTED_EDGE('',*,*,#4463,.T.);
#5943=ORIENTED_EDGE('',*,*,#4464,.T.);
#5944=ORIENTED_EDGE('',*,*,#4465,.T.);
#5945=ORIENTED_EDGE('',*,*,#4461,.F.);
#5946=ORIENTED_EDGE('',*,*,#4466,.T.);
#5947=ORIENTED_EDGE('',*,*,#4467,.T.);
#5948=ORIENTED_EDGE('',*,*,#4468,.T.);
#5949=ORIENTED_EDGE('',*,*,#4464,.F.);
#5950=ORIENTED_EDGE('',*,*,#4469,.T.);
#5951=ORIENTED_EDGE('',*,*,#4470,.T.);
#5952=ORIENTED_EDGE('',*,*,#4471,.T.);
#5953=ORIENTED_EDGE('',*,*,#4467,.F.);
#5954=ORIENTED_EDGE('',*,*,#4472,.T.);
#5955=ORIENTED_EDGE('',*,*,#4473,.F.);
#5956=ORIENTED_EDGE('',*,*,#4474,.F.);
#5957=ORIENTED_EDGE('',*,*,#4475,.T.);
#5958=ORIENTED_EDGE('',*,*,#4476,.T.);
#5959=ORIENTED_EDGE('',*,*,#4477,.T.);
#5960=ORIENTED_EDGE('',*,*,#4478,.F.);
#5961=ORIENTED_EDGE('',*,*,#4479,.F.);
#5962=ORIENTED_EDGE('',*,*,#4480,.T.);
#5963=ORIENTED_EDGE('',*,*,#4481,.T.);
#5964=ORIENTED_EDGE('',*,*,#4476,.F.);
#5965=ORIENTED_EDGE('',*,*,#4482,.F.);
#5966=ORIENTED_EDGE('',*,*,#4483,.T.);
#5967=ORIENTED_EDGE('',*,*,#4484,.T.);
#5968=ORIENTED_EDGE('',*,*,#4480,.F.);
#5969=ORIENTED_EDGE('',*,*,#4485,.F.);
#5970=ORIENTED_EDGE('',*,*,#4486,.T.);
#5971=ORIENTED_EDGE('',*,*,#4487,.T.);
#5972=ORIENTED_EDGE('',*,*,#4483,.F.);
#5973=ORIENTED_EDGE('',*,*,#4488,.F.);
#5974=ORIENTED_EDGE('',*,*,#4489,.T.);
#5975=ORIENTED_EDGE('',*,*,#4490,.T.);
#5976=ORIENTED_EDGE('',*,*,#4486,.F.);
#5977=ORIENTED_EDGE('',*,*,#4491,.F.);
#5978=ORIENTED_EDGE('',*,*,#4492,.T.);
#5979=ORIENTED_EDGE('',*,*,#4493,.T.);
#5980=ORIENTED_EDGE('',*,*,#4489,.F.);
#5981=ORIENTED_EDGE('',*,*,#4494,.F.);
#5982=ORIENTED_EDGE('',*,*,#4495,.T.);
#5983=ORIENTED_EDGE('',*,*,#4496,.T.);
#5984=ORIENTED_EDGE('',*,*,#4492,.F.);
#5985=ORIENTED_EDGE('',*,*,#4497,.F.);
#5986=ORIENTED_EDGE('',*,*,#4498,.T.);
#5987=ORIENTED_EDGE('',*,*,#4499,.T.);
#5988=ORIENTED_EDGE('',*,*,#4495,.F.);
#5989=ORIENTED_EDGE('',*,*,#4500,.F.);
#5990=ORIENTED_EDGE('',*,*,#4501,.F.);
#5991=ORIENTED_EDGE('',*,*,#4502,.F.);
#5992=ORIENTED_EDGE('',*,*,#4503,.F.);
#5993=ORIENTED_EDGE('',*,*,#4504,.T.);
#5994=ORIENTED_EDGE('',*,*,#4501,.T.);
#5995=ORIENTED_EDGE('',*,*,#4505,.T.);
#5996=ORIENTED_EDGE('',*,*,#4498,.F.);
#5997=ORIENTED_EDGE('',*,*,#4506,.F.);
#5998=ORIENTED_EDGE('',*,*,#4507,.F.);
#5999=ORIENTED_EDGE('',*,*,#4477,.F.);
#6000=ORIENTED_EDGE('',*,*,#4481,.F.);
#6001=ORIENTED_EDGE('',*,*,#4484,.F.);
#6002=ORIENTED_EDGE('',*,*,#4487,.F.);
#6003=ORIENTED_EDGE('',*,*,#4490,.F.);
#6004=ORIENTED_EDGE('',*,*,#4493,.F.);
#6005=ORIENTED_EDGE('',*,*,#4496,.F.);
#6006=ORIENTED_EDGE('',*,*,#4499,.F.);
#6007=ORIENTED_EDGE('',*,*,#4505,.F.);
#6008=ORIENTED_EDGE('',*,*,#4504,.F.);
#6009=ORIENTED_EDGE('',*,*,#4508,.F.);
#6010=ORIENTED_EDGE('',*,*,#4449,.F.);
#6011=ORIENTED_EDGE('',*,*,#4453,.F.);
#6012=ORIENTED_EDGE('',*,*,#4456,.F.);
#6013=ORIENTED_EDGE('',*,*,#4459,.F.);
#6014=ORIENTED_EDGE('',*,*,#4462,.F.);
#6015=ORIENTED_EDGE('',*,*,#4465,.F.);
#6016=ORIENTED_EDGE('',*,*,#4468,.F.);
#6017=ORIENTED_EDGE('',*,*,#4471,.F.);
#6018=ORIENTED_EDGE('',*,*,#4509,.F.);
#6019=ORIENTED_EDGE('',*,*,#4475,.F.);
#6020=ORIENTED_EDGE('',*,*,#4510,.F.);
#6021=ORIENTED_EDGE('',*,*,#4511,.F.);
#6022=ORIENTED_EDGE('',*,*,#4472,.F.);
#6023=ORIENTED_EDGE('',*,*,#4469,.F.);
#6024=ORIENTED_EDGE('',*,*,#4466,.F.);
#6025=ORIENTED_EDGE('',*,*,#4463,.F.);
#6026=ORIENTED_EDGE('',*,*,#4460,.F.);
#6027=ORIENTED_EDGE('',*,*,#4457,.F.);
#6028=ORIENTED_EDGE('',*,*,#4454,.F.);
#6029=ORIENTED_EDGE('',*,*,#4451,.F.);
#6030=ORIENTED_EDGE('',*,*,#4512,.F.);
#6031=ORIENTED_EDGE('',*,*,#4502,.T.);
#6032=ORIENTED_EDGE('',*,*,#4506,.T.);
#6033=ORIENTED_EDGE('',*,*,#4500,.T.);
#6034=ORIENTED_EDGE('',*,*,#4497,.T.);
#6035=ORIENTED_EDGE('',*,*,#4494,.T.);
#6036=ORIENTED_EDGE('',*,*,#4491,.T.);
#6037=ORIENTED_EDGE('',*,*,#4488,.T.);
#6038=ORIENTED_EDGE('',*,*,#4485,.T.);
#6039=ORIENTED_EDGE('',*,*,#4482,.T.);
#6040=ORIENTED_EDGE('',*,*,#4479,.T.);
#6041=ORIENTED_EDGE('',*,*,#4513,.T.);
#6042=ORIENTED_EDGE('',*,*,#4514,.T.);
#6043=ORIENTED_EDGE('',*,*,#4510,.T.);
#6044=ORIENTED_EDGE('',*,*,#4478,.T.);
#6045=ORIENTED_EDGE('',*,*,#4507,.T.);
#6046=ORIENTED_EDGE('',*,*,#4474,.T.);
#6047=ORIENTED_EDGE('',*,*,#4515,.T.);
#6048=ORIENTED_EDGE('',*,*,#4516,.T.);
#6049=ORIENTED_EDGE('',*,*,#4517,.T.);
#6050=ORIENTED_EDGE('',*,*,#4518,.T.);
#6051=ORIENTED_EDGE('',*,*,#4519,.F.);
#6052=ORIENTED_EDGE('',*,*,#4520,.T.);
#6053=ORIENTED_EDGE('',*,*,#4518,.F.);
#6054=ORIENTED_EDGE('',*,*,#4520,.F.);
#6055=ORIENTED_EDGE('',*,*,#4521,.F.);
#6056=ORIENTED_EDGE('',*,*,#4522,.T.);
#6057=ORIENTED_EDGE('',*,*,#4517,.F.);
#6058=ORIENTED_EDGE('',*,*,#4522,.F.);
#6059=ORIENTED_EDGE('',*,*,#4523,.F.);
#6060=ORIENTED_EDGE('',*,*,#4524,.T.);
#6061=ORIENTED_EDGE('',*,*,#4516,.F.);
#6062=ORIENTED_EDGE('',*,*,#4524,.F.);
#6063=ORIENTED_EDGE('',*,*,#4525,.F.);
#6064=ORIENTED_EDGE('',*,*,#4526,.F.);
#6065=ORIENTED_EDGE('',*,*,#4513,.F.);
#6066=ORIENTED_EDGE('',*,*,#4527,.F.);
#6067=ORIENTED_EDGE('',*,*,#4525,.T.);
#6068=ORIENTED_EDGE('',*,*,#4528,.F.);
#6069=ORIENTED_EDGE('',*,*,#4519,.T.);
#6070=ORIENTED_EDGE('',*,*,#4521,.T.);
#6071=ORIENTED_EDGE('',*,*,#4523,.T.);
#6072=ORIENTED_EDGE('',*,*,#4529,.T.);
#6073=ORIENTED_EDGE('',*,*,#4527,.T.);
#6074=ORIENTED_EDGE('',*,*,#4514,.F.);
#6075=ORIENTED_EDGE('',*,*,#4526,.T.);
#6076=ORIENTED_EDGE('',*,*,#4528,.T.);
#6077=ORIENTED_EDGE('',*,*,#4473,.T.);
#6078=ORIENTED_EDGE('',*,*,#4509,.T.);
#6079=ORIENTED_EDGE('',*,*,#4470,.F.);
#6080=ORIENTED_EDGE('',*,*,#4511,.T.);
#6081=ORIENTED_EDGE('',*,*,#4515,.F.);
#6082=ORIENTED_EDGE('',*,*,#4529,.F.);
#6083=ORIENTED_EDGE('',*,*,#4530,.T.);
#6084=ORIENTED_EDGE('',*,*,#4531,.T.);
#6085=ORIENTED_EDGE('',*,*,#4530,.F.);
#6086=ORIENTED_EDGE('',*,*,#4531,.F.);
#6087=ORIENTED_EDGE('',*,*,#4512,.T.);
#6088=ORIENTED_EDGE('',*,*,#4450,.F.);
#6089=ORIENTED_EDGE('',*,*,#4508,.T.);
#6090=ORIENTED_EDGE('',*,*,#4503,.T.);
#6091=ORIENTED_EDGE('',*,*,#4532,.F.);
#6092=ORIENTED_EDGE('',*,*,#4533,.F.);
#6093=ORIENTED_EDGE('',*,*,#4534,.T.);
#6094=ORIENTED_EDGE('',*,*,#4532,.T.);
#6095=ORIENTED_EDGE('',*,*,#4534,.F.);
#6096=ORIENTED_EDGE('',*,*,#4535,.F.);
#6097=ORIENTED_EDGE('',*,*,#4536,.T.);
#6098=ORIENTED_EDGE('',*,*,#4533,.T.);
#6099=ORIENTED_EDGE('',*,*,#4536,.F.);
#6100=ORIENTED_EDGE('',*,*,#4537,.F.);
#6101=ORIENTED_EDGE('',*,*,#4538,.T.);
#6102=ORIENTED_EDGE('',*,*,#4535,.T.);
#6103=ORIENTED_EDGE('',*,*,#4538,.F.);
#6104=ORIENTED_EDGE('',*,*,#4537,.T.);
#6105=ORIENTED_EDGE('',*,*,#4539,.F.);
#6106=ORIENTED_EDGE('',*,*,#4540,.F.);
#6107=ORIENTED_EDGE('',*,*,#4541,.T.);
#6108=ORIENTED_EDGE('',*,*,#4539,.T.);
#6109=ORIENTED_EDGE('',*,*,#4541,.F.);
#6110=ORIENTED_EDGE('',*,*,#4542,.F.);
#6111=ORIENTED_EDGE('',*,*,#4543,.T.);
#6112=ORIENTED_EDGE('',*,*,#4540,.T.);
#6113=ORIENTED_EDGE('',*,*,#4543,.F.);
#6114=ORIENTED_EDGE('',*,*,#4544,.F.);
#6115=ORIENTED_EDGE('',*,*,#4545,.T.);
#6116=ORIENTED_EDGE('',*,*,#4542,.T.);
#6117=ORIENTED_EDGE('',*,*,#4545,.F.);
#6118=ORIENTED_EDGE('',*,*,#4544,.T.);
#6119=ORIENTED_EDGE('',*,*,#4546,.T.);
#6120=ORIENTED_EDGE('',*,*,#4547,.T.);
#6121=ORIENTED_EDGE('',*,*,#4548,.T.);
#6122=ORIENTED_EDGE('',*,*,#4549,.F.);
#6123=ORIENTED_EDGE('',*,*,#4550,.T.);
#6124=ORIENTED_EDGE('',*,*,#4551,.T.);
#6125=ORIENTED_EDGE('',*,*,#4552,.T.);
#6126=ORIENTED_EDGE('',*,*,#4547,.F.);
#6127=ORIENTED_EDGE('',*,*,#4553,.T.);
#6128=ORIENTED_EDGE('',*,*,#4554,.T.);
#6129=ORIENTED_EDGE('',*,*,#4555,.T.);
#6130=ORIENTED_EDGE('',*,*,#4551,.F.);
#6131=ORIENTED_EDGE('',*,*,#4556,.T.);
#6132=ORIENTED_EDGE('',*,*,#4557,.T.);
#6133=ORIENTED_EDGE('',*,*,#4558,.T.);
#6134=ORIENTED_EDGE('',*,*,#4554,.F.);
#6135=ORIENTED_EDGE('',*,*,#4559,.T.);
#6136=ORIENTED_EDGE('',*,*,#4560,.T.);
#6137=ORIENTED_EDGE('',*,*,#4561,.T.);
#6138=ORIENTED_EDGE('',*,*,#4557,.F.);
#6139=ORIENTED_EDGE('',*,*,#4562,.T.);
#6140=ORIENTED_EDGE('',*,*,#4549,.T.);
#6141=ORIENTED_EDGE('',*,*,#4563,.T.);
#6142=ORIENTED_EDGE('',*,*,#4560,.F.);
#6143=ORIENTED_EDGE('',*,*,#4562,.F.);
#6144=ORIENTED_EDGE('',*,*,#4559,.F.);
#6145=ORIENTED_EDGE('',*,*,#4556,.F.);
#6146=ORIENTED_EDGE('',*,*,#4553,.F.);
#6147=ORIENTED_EDGE('',*,*,#4550,.F.);
#6148=ORIENTED_EDGE('',*,*,#4546,.F.);
#6149=ORIENTED_EDGE('',*,*,#4563,.F.);
#6150=ORIENTED_EDGE('',*,*,#4548,.F.);
#6151=ORIENTED_EDGE('',*,*,#4552,.F.);
#6152=ORIENTED_EDGE('',*,*,#4555,.F.);
#6153=ORIENTED_EDGE('',*,*,#4558,.F.);
#6154=ORIENTED_EDGE('',*,*,#4561,.F.);
#6155=ORIENTED_EDGE('',*,*,#4564,.F.);
#6156=ORIENTED_EDGE('',*,*,#4565,.F.);
#6157=ORIENTED_EDGE('',*,*,#4566,.T.);
#6158=ORIENTED_EDGE('',*,*,#4564,.T.);
#6159=ORIENTED_EDGE('',*,*,#4566,.F.);
#6160=ORIENTED_EDGE('',*,*,#4567,.F.);
#6161=ORIENTED_EDGE('',*,*,#4568,.T.);
#6162=ORIENTED_EDGE('',*,*,#4565,.T.);
#6163=ORIENTED_EDGE('',*,*,#4568,.F.);
#6164=ORIENTED_EDGE('',*,*,#4569,.F.);
#6165=ORIENTED_EDGE('',*,*,#4570,.T.);
#6166=ORIENTED_EDGE('',*,*,#4567,.T.);
#6167=ORIENTED_EDGE('',*,*,#4570,.F.);
#6168=ORIENTED_EDGE('',*,*,#4569,.T.);
#6169=ORIENTED_EDGE('',*,*,#4571,.F.);
#6170=ORIENTED_EDGE('',*,*,#4572,.F.);
#6171=ORIENTED_EDGE('',*,*,#4573,.T.);
#6172=ORIENTED_EDGE('',*,*,#4571,.T.);
#6173=ORIENTED_EDGE('',*,*,#4573,.F.);
#6174=ORIENTED_EDGE('',*,*,#4574,.F.);
#6175=ORIENTED_EDGE('',*,*,#4575,.T.);
#6176=ORIENTED_EDGE('',*,*,#4572,.T.);
#6177=ORIENTED_EDGE('',*,*,#4575,.F.);
#6178=ORIENTED_EDGE('',*,*,#4576,.F.);
#6179=ORIENTED_EDGE('',*,*,#4577,.T.);
#6180=ORIENTED_EDGE('',*,*,#4574,.T.);
#6181=ORIENTED_EDGE('',*,*,#4577,.F.);
#6182=ORIENTED_EDGE('',*,*,#4576,.T.);
#6183=ORIENTED_EDGE('',*,*,#4578,.T.);
#6184=ORIENTED_EDGE('',*,*,#4579,.T.);
#6185=ORIENTED_EDGE('',*,*,#4580,.T.);
#6186=ORIENTED_EDGE('',*,*,#4581,.F.);
#6187=ORIENTED_EDGE('',*,*,#4582,.T.);
#6188=ORIENTED_EDGE('',*,*,#4583,.T.);
#6189=ORIENTED_EDGE('',*,*,#4584,.T.);
#6190=ORIENTED_EDGE('',*,*,#4579,.F.);
#6191=ORIENTED_EDGE('',*,*,#4585,.T.);
#6192=ORIENTED_EDGE('',*,*,#4586,.T.);
#6193=ORIENTED_EDGE('',*,*,#4587,.T.);
#6194=ORIENTED_EDGE('',*,*,#4583,.F.);
#6195=ORIENTED_EDGE('',*,*,#4588,.T.);
#6196=ORIENTED_EDGE('',*,*,#4589,.T.);
#6197=ORIENTED_EDGE('',*,*,#4590,.T.);
#6198=ORIENTED_EDGE('',*,*,#4586,.F.);
#6199=ORIENTED_EDGE('',*,*,#4591,.T.);
#6200=ORIENTED_EDGE('',*,*,#4592,.T.);
#6201=ORIENTED_EDGE('',*,*,#4593,.T.);
#6202=ORIENTED_EDGE('',*,*,#4589,.F.);
#6203=ORIENTED_EDGE('',*,*,#4594,.T.);
#6204=ORIENTED_EDGE('',*,*,#4581,.T.);
#6205=ORIENTED_EDGE('',*,*,#4595,.T.);
#6206=ORIENTED_EDGE('',*,*,#4592,.F.);
#6207=ORIENTED_EDGE('',*,*,#4594,.F.);
#6208=ORIENTED_EDGE('',*,*,#4591,.F.);
#6209=ORIENTED_EDGE('',*,*,#4588,.F.);
#6210=ORIENTED_EDGE('',*,*,#4585,.F.);
#6211=ORIENTED_EDGE('',*,*,#4582,.F.);
#6212=ORIENTED_EDGE('',*,*,#4578,.F.);
#6213=ORIENTED_EDGE('',*,*,#4595,.F.);
#6214=ORIENTED_EDGE('',*,*,#4580,.F.);
#6215=ORIENTED_EDGE('',*,*,#4584,.F.);
#6216=ORIENTED_EDGE('',*,*,#4587,.F.);
#6217=ORIENTED_EDGE('',*,*,#4590,.F.);
#6218=ORIENTED_EDGE('',*,*,#4593,.F.);
#6219=ORIENTED_EDGE('',*,*,#4596,.F.);
#6220=ORIENTED_EDGE('',*,*,#4597,.T.);
#6221=ORIENTED_EDGE('',*,*,#4598,.T.);
#6222=ORIENTED_EDGE('',*,*,#4599,.T.);
#6223=ORIENTED_EDGE('',*,*,#4600,.F.);
#6224=ORIENTED_EDGE('',*,*,#4601,.T.);
#6225=ORIENTED_EDGE('',*,*,#4596,.T.);
#6226=ORIENTED_EDGE('',*,*,#4602,.T.);
#6227=ORIENTED_EDGE('',*,*,#4603,.F.);
#6228=ORIENTED_EDGE('',*,*,#4604,.T.);
#6229=ORIENTED_EDGE('',*,*,#4600,.T.);
#6230=ORIENTED_EDGE('',*,*,#4605,.T.);
#6231=ORIENTED_EDGE('',*,*,#4606,.F.);
#6232=ORIENTED_EDGE('',*,*,#4607,.T.);
#6233=ORIENTED_EDGE('',*,*,#4603,.T.);
#6234=ORIENTED_EDGE('',*,*,#4608,.T.);
#6235=ORIENTED_EDGE('',*,*,#4609,.F.);
#6236=ORIENTED_EDGE('',*,*,#4610,.T.);
#6237=ORIENTED_EDGE('',*,*,#4606,.T.);
#6238=ORIENTED_EDGE('',*,*,#4611,.T.);
#6239=ORIENTED_EDGE('',*,*,#4612,.F.);
#6240=ORIENTED_EDGE('',*,*,#4613,.T.);
#6241=ORIENTED_EDGE('',*,*,#4609,.T.);
#6242=ORIENTED_EDGE('',*,*,#4614,.T.);
#6243=ORIENTED_EDGE('',*,*,#4615,.F.);
#6244=ORIENTED_EDGE('',*,*,#4616,.T.);
#6245=ORIENTED_EDGE('',*,*,#4612,.T.);
#6246=ORIENTED_EDGE('',*,*,#4617,.T.);
#6247=ORIENTED_EDGE('',*,*,#4618,.F.);
#6248=ORIENTED_EDGE('',*,*,#4619,.T.);
#6249=ORIENTED_EDGE('',*,*,#4615,.T.);
#6250=ORIENTED_EDGE('',*,*,#4620,.T.);
#6251=ORIENTED_EDGE('',*,*,#4621,.F.);
#6252=ORIENTED_EDGE('',*,*,#4622,.T.);
#6253=ORIENTED_EDGE('',*,*,#4618,.T.);
#6254=ORIENTED_EDGE('',*,*,#4623,.T.);
#6255=ORIENTED_EDGE('',*,*,#4624,.F.);
#6256=ORIENTED_EDGE('',*,*,#4625,.T.);
#6257=ORIENTED_EDGE('',*,*,#4621,.T.);
#6258=ORIENTED_EDGE('',*,*,#4626,.T.);
#6259=ORIENTED_EDGE('',*,*,#4627,.F.);
#6260=ORIENTED_EDGE('',*,*,#4628,.T.);
#6261=ORIENTED_EDGE('',*,*,#4624,.T.);
#6262=ORIENTED_EDGE('',*,*,#4629,.T.);
#6263=ORIENTED_EDGE('',*,*,#4630,.F.);
#6264=ORIENTED_EDGE('',*,*,#4631,.T.);
#6265=ORIENTED_EDGE('',*,*,#4627,.T.);
#6266=ORIENTED_EDGE('',*,*,#4632,.T.);
#6267=ORIENTED_EDGE('',*,*,#4633,.F.);
#6268=ORIENTED_EDGE('',*,*,#4634,.T.);
#6269=ORIENTED_EDGE('',*,*,#4630,.T.);
#6270=ORIENTED_EDGE('',*,*,#4635,.T.);
#6271=ORIENTED_EDGE('',*,*,#4636,.F.);
#6272=ORIENTED_EDGE('',*,*,#4637,.T.);
#6273=ORIENTED_EDGE('',*,*,#4633,.T.);
#6274=ORIENTED_EDGE('',*,*,#4638,.T.);
#6275=ORIENTED_EDGE('',*,*,#4639,.F.);
#6276=ORIENTED_EDGE('',*,*,#4640,.T.);
#6277=ORIENTED_EDGE('',*,*,#4636,.T.);
#6278=ORIENTED_EDGE('',*,*,#4641,.T.);
#6279=ORIENTED_EDGE('',*,*,#4642,.F.);
#6280=ORIENTED_EDGE('',*,*,#4643,.T.);
#6281=ORIENTED_EDGE('',*,*,#4639,.T.);
#6282=ORIENTED_EDGE('',*,*,#4644,.T.);
#6283=ORIENTED_EDGE('',*,*,#4645,.F.);
#6284=ORIENTED_EDGE('',*,*,#4646,.T.);
#6285=ORIENTED_EDGE('',*,*,#4642,.T.);
#6286=ORIENTED_EDGE('',*,*,#4647,.T.);
#6287=ORIENTED_EDGE('',*,*,#4648,.F.);
#6288=ORIENTED_EDGE('',*,*,#4649,.T.);
#6289=ORIENTED_EDGE('',*,*,#4645,.T.);
#6290=ORIENTED_EDGE('',*,*,#4650,.T.);
#6291=ORIENTED_EDGE('',*,*,#4651,.F.);
#6292=ORIENTED_EDGE('',*,*,#4652,.T.);
#6293=ORIENTED_EDGE('',*,*,#4648,.T.);
#6294=ORIENTED_EDGE('',*,*,#4653,.T.);
#6295=ORIENTED_EDGE('',*,*,#4654,.F.);
#6296=ORIENTED_EDGE('',*,*,#4655,.T.);
#6297=ORIENTED_EDGE('',*,*,#4651,.T.);
#6298=ORIENTED_EDGE('',*,*,#4656,.T.);
#6299=ORIENTED_EDGE('',*,*,#4657,.F.);
#6300=ORIENTED_EDGE('',*,*,#4658,.T.);
#6301=ORIENTED_EDGE('',*,*,#4654,.T.);
#6302=ORIENTED_EDGE('',*,*,#4659,.T.);
#6303=ORIENTED_EDGE('',*,*,#4660,.F.);
#6304=ORIENTED_EDGE('',*,*,#4661,.T.);
#6305=ORIENTED_EDGE('',*,*,#4657,.T.);
#6306=ORIENTED_EDGE('',*,*,#4662,.T.);
#6307=ORIENTED_EDGE('',*,*,#4663,.F.);
#6308=ORIENTED_EDGE('',*,*,#4664,.T.);
#6309=ORIENTED_EDGE('',*,*,#4660,.T.);
#6310=ORIENTED_EDGE('',*,*,#4665,.T.);
#6311=ORIENTED_EDGE('',*,*,#4666,.F.);
#6312=ORIENTED_EDGE('',*,*,#4667,.T.);
#6313=ORIENTED_EDGE('',*,*,#4663,.T.);
#6314=ORIENTED_EDGE('',*,*,#4668,.T.);
#6315=ORIENTED_EDGE('',*,*,#4669,.F.);
#6316=ORIENTED_EDGE('',*,*,#4670,.T.);
#6317=ORIENTED_EDGE('',*,*,#4666,.T.);
#6318=ORIENTED_EDGE('',*,*,#4671,.T.);
#6319=ORIENTED_EDGE('',*,*,#4672,.F.);
#6320=ORIENTED_EDGE('',*,*,#4673,.T.);
#6321=ORIENTED_EDGE('',*,*,#4669,.T.);
#6322=ORIENTED_EDGE('',*,*,#4674,.T.);
#6323=ORIENTED_EDGE('',*,*,#4675,.F.);
#6324=ORIENTED_EDGE('',*,*,#4676,.T.);
#6325=ORIENTED_EDGE('',*,*,#4672,.T.);
#6326=ORIENTED_EDGE('',*,*,#4677,.T.);
#6327=ORIENTED_EDGE('',*,*,#4678,.F.);
#6328=ORIENTED_EDGE('',*,*,#4679,.T.);
#6329=ORIENTED_EDGE('',*,*,#4675,.T.);
#6330=ORIENTED_EDGE('',*,*,#4680,.T.);
#6331=ORIENTED_EDGE('',*,*,#4681,.F.);
#6332=ORIENTED_EDGE('',*,*,#4682,.T.);
#6333=ORIENTED_EDGE('',*,*,#4678,.T.);
#6334=ORIENTED_EDGE('',*,*,#4683,.T.);
#6335=ORIENTED_EDGE('',*,*,#4684,.F.);
#6336=ORIENTED_EDGE('',*,*,#4685,.T.);
#6337=ORIENTED_EDGE('',*,*,#4681,.T.);
#6338=ORIENTED_EDGE('',*,*,#4686,.T.);
#6339=ORIENTED_EDGE('',*,*,#4687,.F.);
#6340=ORIENTED_EDGE('',*,*,#4688,.T.);
#6341=ORIENTED_EDGE('',*,*,#4684,.T.);
#6342=ORIENTED_EDGE('',*,*,#4689,.T.);
#6343=ORIENTED_EDGE('',*,*,#4690,.F.);
#6344=ORIENTED_EDGE('',*,*,#4691,.T.);
#6345=ORIENTED_EDGE('',*,*,#4687,.T.);
#6346=ORIENTED_EDGE('',*,*,#4692,.T.);
#6347=ORIENTED_EDGE('',*,*,#4693,.F.);
#6348=ORIENTED_EDGE('',*,*,#4694,.T.);
#6349=ORIENTED_EDGE('',*,*,#4690,.T.);
#6350=ORIENTED_EDGE('',*,*,#4695,.T.);
#6351=ORIENTED_EDGE('',*,*,#4696,.F.);
#6352=ORIENTED_EDGE('',*,*,#4697,.T.);
#6353=ORIENTED_EDGE('',*,*,#4693,.T.);
#6354=ORIENTED_EDGE('',*,*,#4698,.T.);
#6355=ORIENTED_EDGE('',*,*,#4699,.F.);
#6356=ORIENTED_EDGE('',*,*,#4700,.T.);
#6357=ORIENTED_EDGE('',*,*,#4696,.T.);
#6358=ORIENTED_EDGE('',*,*,#4701,.T.);
#6359=ORIENTED_EDGE('',*,*,#4702,.F.);
#6360=ORIENTED_EDGE('',*,*,#4703,.T.);
#6361=ORIENTED_EDGE('',*,*,#4699,.T.);
#6362=ORIENTED_EDGE('',*,*,#4704,.T.);
#6363=ORIENTED_EDGE('',*,*,#4705,.F.);
#6364=ORIENTED_EDGE('',*,*,#4706,.T.);
#6365=ORIENTED_EDGE('',*,*,#4702,.T.);
#6366=ORIENTED_EDGE('',*,*,#4707,.T.);
#6367=ORIENTED_EDGE('',*,*,#4708,.F.);
#6368=ORIENTED_EDGE('',*,*,#4709,.T.);
#6369=ORIENTED_EDGE('',*,*,#4705,.T.);
#6370=ORIENTED_EDGE('',*,*,#4710,.T.);
#6371=ORIENTED_EDGE('',*,*,#4711,.F.);
#6372=ORIENTED_EDGE('',*,*,#4712,.T.);
#6373=ORIENTED_EDGE('',*,*,#4708,.T.);
#6374=ORIENTED_EDGE('',*,*,#4713,.T.);
#6375=ORIENTED_EDGE('',*,*,#4714,.F.);
#6376=ORIENTED_EDGE('',*,*,#4715,.T.);
#6377=ORIENTED_EDGE('',*,*,#4711,.T.);
#6378=ORIENTED_EDGE('',*,*,#4716,.T.);
#6379=ORIENTED_EDGE('',*,*,#4717,.F.);
#6380=ORIENTED_EDGE('',*,*,#4718,.T.);
#6381=ORIENTED_EDGE('',*,*,#4714,.T.);
#6382=ORIENTED_EDGE('',*,*,#4719,.T.);
#6383=ORIENTED_EDGE('',*,*,#4720,.F.);
#6384=ORIENTED_EDGE('',*,*,#4721,.T.);
#6385=ORIENTED_EDGE('',*,*,#4717,.T.);
#6386=ORIENTED_EDGE('',*,*,#4722,.T.);
#6387=ORIENTED_EDGE('',*,*,#4723,.F.);
#6388=ORIENTED_EDGE('',*,*,#4724,.T.);
#6389=ORIENTED_EDGE('',*,*,#4720,.T.);
#6390=ORIENTED_EDGE('',*,*,#4725,.T.);
#6391=ORIENTED_EDGE('',*,*,#4726,.F.);
#6392=ORIENTED_EDGE('',*,*,#4727,.T.);
#6393=ORIENTED_EDGE('',*,*,#4723,.T.);
#6394=ORIENTED_EDGE('',*,*,#4728,.T.);
#6395=ORIENTED_EDGE('',*,*,#4729,.F.);
#6396=ORIENTED_EDGE('',*,*,#4730,.T.);
#6397=ORIENTED_EDGE('',*,*,#4726,.T.);
#6398=ORIENTED_EDGE('',*,*,#4731,.T.);
#6399=ORIENTED_EDGE('',*,*,#4732,.F.);
#6400=ORIENTED_EDGE('',*,*,#4733,.T.);
#6401=ORIENTED_EDGE('',*,*,#4729,.T.);
#6402=ORIENTED_EDGE('',*,*,#4734,.T.);
#6403=ORIENTED_EDGE('',*,*,#4735,.F.);
#6404=ORIENTED_EDGE('',*,*,#4736,.T.);
#6405=ORIENTED_EDGE('',*,*,#4732,.T.);
#6406=ORIENTED_EDGE('',*,*,#4737,.T.);
#6407=ORIENTED_EDGE('',*,*,#4738,.F.);
#6408=ORIENTED_EDGE('',*,*,#4739,.T.);
#6409=ORIENTED_EDGE('',*,*,#4735,.T.);
#6410=ORIENTED_EDGE('',*,*,#4740,.T.);
#6411=ORIENTED_EDGE('',*,*,#4741,.F.);
#6412=ORIENTED_EDGE('',*,*,#4742,.T.);
#6413=ORIENTED_EDGE('',*,*,#4738,.T.);
#6414=ORIENTED_EDGE('',*,*,#4743,.T.);
#6415=ORIENTED_EDGE('',*,*,#4744,.F.);
#6416=ORIENTED_EDGE('',*,*,#4745,.T.);
#6417=ORIENTED_EDGE('',*,*,#4741,.T.);
#6418=ORIENTED_EDGE('',*,*,#4746,.T.);
#6419=ORIENTED_EDGE('',*,*,#4747,.F.);
#6420=ORIENTED_EDGE('',*,*,#4748,.T.);
#6421=ORIENTED_EDGE('',*,*,#4744,.T.);
#6422=ORIENTED_EDGE('',*,*,#4749,.T.);
#6423=ORIENTED_EDGE('',*,*,#4750,.F.);
#6424=ORIENTED_EDGE('',*,*,#4751,.T.);
#6425=ORIENTED_EDGE('',*,*,#4747,.T.);
#6426=ORIENTED_EDGE('',*,*,#4752,.T.);
#6427=ORIENTED_EDGE('',*,*,#4753,.F.);
#6428=ORIENTED_EDGE('',*,*,#4754,.T.);
#6429=ORIENTED_EDGE('',*,*,#4750,.T.);
#6430=ORIENTED_EDGE('',*,*,#4755,.T.);
#6431=ORIENTED_EDGE('',*,*,#4756,.F.);
#6432=ORIENTED_EDGE('',*,*,#4757,.T.);
#6433=ORIENTED_EDGE('',*,*,#4753,.T.);
#6434=ORIENTED_EDGE('',*,*,#4758,.T.);
#6435=ORIENTED_EDGE('',*,*,#4759,.F.);
#6436=ORIENTED_EDGE('',*,*,#4760,.T.);
#6437=ORIENTED_EDGE('',*,*,#4756,.T.);
#6438=ORIENTED_EDGE('',*,*,#4761,.T.);
#6439=ORIENTED_EDGE('',*,*,#4762,.F.);
#6440=ORIENTED_EDGE('',*,*,#4763,.T.);
#6441=ORIENTED_EDGE('',*,*,#4759,.T.);
#6442=ORIENTED_EDGE('',*,*,#4764,.T.);
#6443=ORIENTED_EDGE('',*,*,#4765,.F.);
#6444=ORIENTED_EDGE('',*,*,#4766,.T.);
#6445=ORIENTED_EDGE('',*,*,#4762,.T.);
#6446=ORIENTED_EDGE('',*,*,#4767,.T.);
#6447=ORIENTED_EDGE('',*,*,#4768,.F.);
#6448=ORIENTED_EDGE('',*,*,#4769,.T.);
#6449=ORIENTED_EDGE('',*,*,#4765,.T.);
#6450=ORIENTED_EDGE('',*,*,#4770,.T.);
#6451=ORIENTED_EDGE('',*,*,#4771,.F.);
#6452=ORIENTED_EDGE('',*,*,#4772,.T.);
#6453=ORIENTED_EDGE('',*,*,#4768,.T.);
#6454=ORIENTED_EDGE('',*,*,#4773,.T.);
#6455=ORIENTED_EDGE('',*,*,#4774,.F.);
#6456=ORIENTED_EDGE('',*,*,#4775,.T.);
#6457=ORIENTED_EDGE('',*,*,#4771,.T.);
#6458=ORIENTED_EDGE('',*,*,#4776,.T.);
#6459=ORIENTED_EDGE('',*,*,#4777,.F.);
#6460=ORIENTED_EDGE('',*,*,#4778,.T.);
#6461=ORIENTED_EDGE('',*,*,#4774,.T.);
#6462=ORIENTED_EDGE('',*,*,#4779,.T.);
#6463=ORIENTED_EDGE('',*,*,#4780,.F.);
#6464=ORIENTED_EDGE('',*,*,#4781,.T.);
#6465=ORIENTED_EDGE('',*,*,#4777,.T.);
#6466=ORIENTED_EDGE('',*,*,#4782,.T.);
#6467=ORIENTED_EDGE('',*,*,#4783,.F.);
#6468=ORIENTED_EDGE('',*,*,#4784,.T.);
#6469=ORIENTED_EDGE('',*,*,#4780,.T.);
#6470=ORIENTED_EDGE('',*,*,#4785,.T.);
#6471=ORIENTED_EDGE('',*,*,#4786,.F.);
#6472=ORIENTED_EDGE('',*,*,#4787,.T.);
#6473=ORIENTED_EDGE('',*,*,#4788,.F.);
#6474=ORIENTED_EDGE('',*,*,#4789,.F.);
#6475=ORIENTED_EDGE('',*,*,#4790,.T.);
#6476=ORIENTED_EDGE('',*,*,#4786,.T.);
#6477=ORIENTED_EDGE('',*,*,#4791,.F.);
#6478=ORIENTED_EDGE('',*,*,#4792,.F.);
#6479=ORIENTED_EDGE('',*,*,#4793,.F.);
#6480=ORIENTED_EDGE('',*,*,#4794,.T.);
#6481=ORIENTED_EDGE('',*,*,#4789,.T.);
#6482=ORIENTED_EDGE('',*,*,#4795,.F.);
#6483=ORIENTED_EDGE('',*,*,#4796,.F.);
#6484=ORIENTED_EDGE('',*,*,#4797,.T.);
#6485=ORIENTED_EDGE('',*,*,#4793,.T.);
#6486=ORIENTED_EDGE('',*,*,#4798,.F.);
#6487=ORIENTED_EDGE('',*,*,#4799,.F.);
#6488=ORIENTED_EDGE('',*,*,#4800,.T.);
#6489=ORIENTED_EDGE('',*,*,#4796,.T.);
#6490=ORIENTED_EDGE('',*,*,#4801,.F.);
#6491=ORIENTED_EDGE('',*,*,#4802,.F.);
#6492=ORIENTED_EDGE('',*,*,#4803,.T.);
#6493=ORIENTED_EDGE('',*,*,#4799,.T.);
#6494=ORIENTED_EDGE('',*,*,#4804,.F.);
#6495=ORIENTED_EDGE('',*,*,#4805,.F.);
#6496=ORIENTED_EDGE('',*,*,#4806,.T.);
#6497=ORIENTED_EDGE('',*,*,#4802,.T.);
#6498=ORIENTED_EDGE('',*,*,#4807,.F.);
#6499=ORIENTED_EDGE('',*,*,#4808,.F.);
#6500=ORIENTED_EDGE('',*,*,#4809,.T.);
#6501=ORIENTED_EDGE('',*,*,#4805,.T.);
#6502=ORIENTED_EDGE('',*,*,#4810,.F.);
#6503=ORIENTED_EDGE('',*,*,#4811,.F.);
#6504=ORIENTED_EDGE('',*,*,#4812,.T.);
#6505=ORIENTED_EDGE('',*,*,#4808,.T.);
#6506=ORIENTED_EDGE('',*,*,#4813,.F.);
#6507=ORIENTED_EDGE('',*,*,#4814,.F.);
#6508=ORIENTED_EDGE('',*,*,#4815,.T.);
#6509=ORIENTED_EDGE('',*,*,#4811,.T.);
#6510=ORIENTED_EDGE('',*,*,#4816,.F.);
#6511=ORIENTED_EDGE('',*,*,#4817,.F.);
#6512=ORIENTED_EDGE('',*,*,#4818,.T.);
#6513=ORIENTED_EDGE('',*,*,#4814,.T.);
#6514=ORIENTED_EDGE('',*,*,#4819,.F.);
#6515=ORIENTED_EDGE('',*,*,#4820,.F.);
#6516=ORIENTED_EDGE('',*,*,#4821,.T.);
#6517=ORIENTED_EDGE('',*,*,#4817,.T.);
#6518=ORIENTED_EDGE('',*,*,#4822,.F.);
#6519=ORIENTED_EDGE('',*,*,#4823,.F.);
#6520=ORIENTED_EDGE('',*,*,#4824,.T.);
#6521=ORIENTED_EDGE('',*,*,#4820,.T.);
#6522=ORIENTED_EDGE('',*,*,#4825,.F.);
#6523=ORIENTED_EDGE('',*,*,#4826,.F.);
#6524=ORIENTED_EDGE('',*,*,#4827,.T.);
#6525=ORIENTED_EDGE('',*,*,#4823,.T.);
#6526=ORIENTED_EDGE('',*,*,#4828,.F.);
#6527=ORIENTED_EDGE('',*,*,#4829,.F.);
#6528=ORIENTED_EDGE('',*,*,#4830,.T.);
#6529=ORIENTED_EDGE('',*,*,#4826,.T.);
#6530=ORIENTED_EDGE('',*,*,#4831,.F.);
#6531=ORIENTED_EDGE('',*,*,#4832,.F.);
#6532=ORIENTED_EDGE('',*,*,#4833,.T.);
#6533=ORIENTED_EDGE('',*,*,#4829,.T.);
#6534=ORIENTED_EDGE('',*,*,#4834,.F.);
#6535=ORIENTED_EDGE('',*,*,#4835,.F.);
#6536=ORIENTED_EDGE('',*,*,#4836,.T.);
#6537=ORIENTED_EDGE('',*,*,#4832,.T.);
#6538=ORIENTED_EDGE('',*,*,#4837,.F.);
#6539=ORIENTED_EDGE('',*,*,#4838,.F.);
#6540=ORIENTED_EDGE('',*,*,#4839,.T.);
#6541=ORIENTED_EDGE('',*,*,#4835,.T.);
#6542=ORIENTED_EDGE('',*,*,#4840,.F.);
#6543=ORIENTED_EDGE('',*,*,#4841,.F.);
#6544=ORIENTED_EDGE('',*,*,#4842,.T.);
#6545=ORIENTED_EDGE('',*,*,#4838,.T.);
#6546=ORIENTED_EDGE('',*,*,#4843,.F.);
#6547=ORIENTED_EDGE('',*,*,#4844,.F.);
#6548=ORIENTED_EDGE('',*,*,#4845,.T.);
#6549=ORIENTED_EDGE('',*,*,#4841,.T.);
#6550=ORIENTED_EDGE('',*,*,#4846,.F.);
#6551=ORIENTED_EDGE('',*,*,#4847,.F.);
#6552=ORIENTED_EDGE('',*,*,#4848,.T.);
#6553=ORIENTED_EDGE('',*,*,#4844,.T.);
#6554=ORIENTED_EDGE('',*,*,#4849,.F.);
#6555=ORIENTED_EDGE('',*,*,#4850,.F.);
#6556=ORIENTED_EDGE('',*,*,#4851,.T.);
#6557=ORIENTED_EDGE('',*,*,#4847,.T.);
#6558=ORIENTED_EDGE('',*,*,#4852,.F.);
#6559=ORIENTED_EDGE('',*,*,#4853,.F.);
#6560=ORIENTED_EDGE('',*,*,#4854,.T.);
#6561=ORIENTED_EDGE('',*,*,#4850,.T.);
#6562=ORIENTED_EDGE('',*,*,#4855,.F.);
#6563=ORIENTED_EDGE('',*,*,#4856,.F.);
#6564=ORIENTED_EDGE('',*,*,#4857,.T.);
#6565=ORIENTED_EDGE('',*,*,#4853,.T.);
#6566=ORIENTED_EDGE('',*,*,#4858,.F.);
#6567=ORIENTED_EDGE('',*,*,#4859,.F.);
#6568=ORIENTED_EDGE('',*,*,#4860,.T.);
#6569=ORIENTED_EDGE('',*,*,#4856,.T.);
#6570=ORIENTED_EDGE('',*,*,#4861,.F.);
#6571=ORIENTED_EDGE('',*,*,#4862,.F.);
#6572=ORIENTED_EDGE('',*,*,#4863,.T.);
#6573=ORIENTED_EDGE('',*,*,#4859,.T.);
#6574=ORIENTED_EDGE('',*,*,#4864,.F.);
#6575=ORIENTED_EDGE('',*,*,#4865,.F.);
#6576=ORIENTED_EDGE('',*,*,#4866,.T.);
#6577=ORIENTED_EDGE('',*,*,#4862,.T.);
#6578=ORIENTED_EDGE('',*,*,#4867,.F.);
#6579=ORIENTED_EDGE('',*,*,#4868,.F.);
#6580=ORIENTED_EDGE('',*,*,#4869,.T.);
#6581=ORIENTED_EDGE('',*,*,#4865,.T.);
#6582=ORIENTED_EDGE('',*,*,#4870,.F.);
#6583=ORIENTED_EDGE('',*,*,#4871,.F.);
#6584=ORIENTED_EDGE('',*,*,#4872,.T.);
#6585=ORIENTED_EDGE('',*,*,#4868,.T.);
#6586=ORIENTED_EDGE('',*,*,#4873,.F.);
#6587=ORIENTED_EDGE('',*,*,#4874,.F.);
#6588=ORIENTED_EDGE('',*,*,#4875,.T.);
#6589=ORIENTED_EDGE('',*,*,#4871,.T.);
#6590=ORIENTED_EDGE('',*,*,#4876,.F.);
#6591=ORIENTED_EDGE('',*,*,#4877,.F.);
#6592=ORIENTED_EDGE('',*,*,#4878,.T.);
#6593=ORIENTED_EDGE('',*,*,#4874,.T.);
#6594=ORIENTED_EDGE('',*,*,#4879,.F.);
#6595=ORIENTED_EDGE('',*,*,#4880,.F.);
#6596=ORIENTED_EDGE('',*,*,#4881,.T.);
#6597=ORIENTED_EDGE('',*,*,#4877,.T.);
#6598=ORIENTED_EDGE('',*,*,#4882,.F.);
#6599=ORIENTED_EDGE('',*,*,#4883,.F.);
#6600=ORIENTED_EDGE('',*,*,#4884,.T.);
#6601=ORIENTED_EDGE('',*,*,#4880,.T.);
#6602=ORIENTED_EDGE('',*,*,#4885,.F.);
#6603=ORIENTED_EDGE('',*,*,#4886,.F.);
#6604=ORIENTED_EDGE('',*,*,#4887,.T.);
#6605=ORIENTED_EDGE('',*,*,#4883,.T.);
#6606=ORIENTED_EDGE('',*,*,#4888,.F.);
#6607=ORIENTED_EDGE('',*,*,#4889,.F.);
#6608=ORIENTED_EDGE('',*,*,#4890,.T.);
#6609=ORIENTED_EDGE('',*,*,#4886,.T.);
#6610=ORIENTED_EDGE('',*,*,#4891,.F.);
#6611=ORIENTED_EDGE('',*,*,#4892,.F.);
#6612=ORIENTED_EDGE('',*,*,#4893,.T.);
#6613=ORIENTED_EDGE('',*,*,#4889,.T.);
#6614=ORIENTED_EDGE('',*,*,#4894,.F.);
#6615=ORIENTED_EDGE('',*,*,#4895,.F.);
#6616=ORIENTED_EDGE('',*,*,#4896,.T.);
#6617=ORIENTED_EDGE('',*,*,#4892,.T.);
#6618=ORIENTED_EDGE('',*,*,#4897,.F.);
#6619=ORIENTED_EDGE('',*,*,#4898,.F.);
#6620=ORIENTED_EDGE('',*,*,#4899,.T.);
#6621=ORIENTED_EDGE('',*,*,#4895,.T.);
#6622=ORIENTED_EDGE('',*,*,#4900,.F.);
#6623=ORIENTED_EDGE('',*,*,#4901,.F.);
#6624=ORIENTED_EDGE('',*,*,#4902,.T.);
#6625=ORIENTED_EDGE('',*,*,#4898,.T.);
#6626=ORIENTED_EDGE('',*,*,#4903,.F.);
#6627=ORIENTED_EDGE('',*,*,#4904,.F.);
#6628=ORIENTED_EDGE('',*,*,#4905,.T.);
#6629=ORIENTED_EDGE('',*,*,#4901,.T.);
#6630=ORIENTED_EDGE('',*,*,#4906,.F.);
#6631=ORIENTED_EDGE('',*,*,#4907,.F.);
#6632=ORIENTED_EDGE('',*,*,#4908,.T.);
#6633=ORIENTED_EDGE('',*,*,#4904,.T.);
#6634=ORIENTED_EDGE('',*,*,#4909,.F.);
#6635=ORIENTED_EDGE('',*,*,#4910,.F.);
#6636=ORIENTED_EDGE('',*,*,#4911,.T.);
#6637=ORIENTED_EDGE('',*,*,#4907,.T.);
#6638=ORIENTED_EDGE('',*,*,#4912,.F.);
#6639=ORIENTED_EDGE('',*,*,#4913,.F.);
#6640=ORIENTED_EDGE('',*,*,#4914,.T.);
#6641=ORIENTED_EDGE('',*,*,#4910,.T.);
#6642=ORIENTED_EDGE('',*,*,#4915,.F.);
#6643=ORIENTED_EDGE('',*,*,#4916,.F.);
#6644=ORIENTED_EDGE('',*,*,#4917,.T.);
#6645=ORIENTED_EDGE('',*,*,#4913,.T.);
#6646=ORIENTED_EDGE('',*,*,#4918,.F.);
#6647=ORIENTED_EDGE('',*,*,#4919,.F.);
#6648=ORIENTED_EDGE('',*,*,#4920,.T.);
#6649=ORIENTED_EDGE('',*,*,#4916,.T.);
#6650=ORIENTED_EDGE('',*,*,#4921,.F.);
#6651=ORIENTED_EDGE('',*,*,#4922,.F.);
#6652=ORIENTED_EDGE('',*,*,#4923,.T.);
#6653=ORIENTED_EDGE('',*,*,#4919,.T.);
#6654=ORIENTED_EDGE('',*,*,#4924,.F.);
#6655=ORIENTED_EDGE('',*,*,#4925,.F.);
#6656=ORIENTED_EDGE('',*,*,#4926,.T.);
#6657=ORIENTED_EDGE('',*,*,#4922,.T.);
#6658=ORIENTED_EDGE('',*,*,#4927,.F.);
#6659=ORIENTED_EDGE('',*,*,#4928,.F.);
#6660=ORIENTED_EDGE('',*,*,#4929,.T.);
#6661=ORIENTED_EDGE('',*,*,#4925,.T.);
#6662=ORIENTED_EDGE('',*,*,#4930,.F.);
#6663=ORIENTED_EDGE('',*,*,#4931,.F.);
#6664=ORIENTED_EDGE('',*,*,#4932,.T.);
#6665=ORIENTED_EDGE('',*,*,#4928,.T.);
#6666=ORIENTED_EDGE('',*,*,#4933,.F.);
#6667=ORIENTED_EDGE('',*,*,#4934,.F.);
#6668=ORIENTED_EDGE('',*,*,#4935,.T.);
#6669=ORIENTED_EDGE('',*,*,#4931,.T.);
#6670=ORIENTED_EDGE('',*,*,#4936,.F.);
#6671=ORIENTED_EDGE('',*,*,#4937,.F.);
#6672=ORIENTED_EDGE('',*,*,#4938,.T.);
#6673=ORIENTED_EDGE('',*,*,#4934,.T.);
#6674=ORIENTED_EDGE('',*,*,#4939,.F.);
#6675=ORIENTED_EDGE('',*,*,#4940,.F.);
#6676=ORIENTED_EDGE('',*,*,#4941,.T.);
#6677=ORIENTED_EDGE('',*,*,#4937,.T.);
#6678=ORIENTED_EDGE('',*,*,#4942,.F.);
#6679=ORIENTED_EDGE('',*,*,#4943,.F.);
#6680=ORIENTED_EDGE('',*,*,#4944,.T.);
#6681=ORIENTED_EDGE('',*,*,#4940,.T.);
#6682=ORIENTED_EDGE('',*,*,#4945,.F.);
#6683=ORIENTED_EDGE('',*,*,#4946,.F.);
#6684=ORIENTED_EDGE('',*,*,#4947,.T.);
#6685=ORIENTED_EDGE('',*,*,#4943,.T.);
#6686=ORIENTED_EDGE('',*,*,#4948,.F.);
#6687=ORIENTED_EDGE('',*,*,#4949,.F.);
#6688=ORIENTED_EDGE('',*,*,#4950,.T.);
#6689=ORIENTED_EDGE('',*,*,#4946,.T.);
#6690=ORIENTED_EDGE('',*,*,#4951,.F.);
#6691=ORIENTED_EDGE('',*,*,#4952,.F.);
#6692=ORIENTED_EDGE('',*,*,#4953,.T.);
#6693=ORIENTED_EDGE('',*,*,#4949,.T.);
#6694=ORIENTED_EDGE('',*,*,#4954,.F.);
#6695=ORIENTED_EDGE('',*,*,#4955,.F.);
#6696=ORIENTED_EDGE('',*,*,#4956,.T.);
#6697=ORIENTED_EDGE('',*,*,#4952,.T.);
#6698=ORIENTED_EDGE('',*,*,#4957,.F.);
#6699=ORIENTED_EDGE('',*,*,#4958,.F.);
#6700=ORIENTED_EDGE('',*,*,#4959,.T.);
#6701=ORIENTED_EDGE('',*,*,#4955,.T.);
#6702=ORIENTED_EDGE('',*,*,#4960,.F.);
#6703=ORIENTED_EDGE('',*,*,#4961,.F.);
#6704=ORIENTED_EDGE('',*,*,#4962,.T.);
#6705=ORIENTED_EDGE('',*,*,#4958,.T.);
#6706=ORIENTED_EDGE('',*,*,#4963,.F.);
#6707=ORIENTED_EDGE('',*,*,#4964,.F.);
#6708=ORIENTED_EDGE('',*,*,#4965,.T.);
#6709=ORIENTED_EDGE('',*,*,#4961,.T.);
#6710=ORIENTED_EDGE('',*,*,#4966,.F.);
#6711=ORIENTED_EDGE('',*,*,#4967,.F.);
#6712=ORIENTED_EDGE('',*,*,#4968,.T.);
#6713=ORIENTED_EDGE('',*,*,#4964,.T.);
#6714=ORIENTED_EDGE('',*,*,#4969,.F.);
#6715=ORIENTED_EDGE('',*,*,#4970,.F.);
#6716=ORIENTED_EDGE('',*,*,#4971,.T.);
#6717=ORIENTED_EDGE('',*,*,#4967,.T.);
#6718=ORIENTED_EDGE('',*,*,#4972,.F.);
#6719=ORIENTED_EDGE('',*,*,#4973,.F.);
#6720=ORIENTED_EDGE('',*,*,#4974,.T.);
#6721=ORIENTED_EDGE('',*,*,#4970,.T.);
#6722=ORIENTED_EDGE('',*,*,#4975,.F.);
#6723=ORIENTED_EDGE('',*,*,#4976,.F.);
#6724=ORIENTED_EDGE('',*,*,#4977,.F.);
#6725=ORIENTED_EDGE('',*,*,#4785,.F.);
#6726=ORIENTED_EDGE('',*,*,#4782,.F.);
#6727=ORIENTED_EDGE('',*,*,#4779,.F.);
#6728=ORIENTED_EDGE('',*,*,#4776,.F.);
#6729=ORIENTED_EDGE('',*,*,#4773,.F.);
#6730=ORIENTED_EDGE('',*,*,#4770,.F.);
#6731=ORIENTED_EDGE('',*,*,#4767,.F.);
#6732=ORIENTED_EDGE('',*,*,#4764,.F.);
#6733=ORIENTED_EDGE('',*,*,#4761,.F.);
#6734=ORIENTED_EDGE('',*,*,#4758,.F.);
#6735=ORIENTED_EDGE('',*,*,#4755,.F.);
#6736=ORIENTED_EDGE('',*,*,#4752,.F.);
#6737=ORIENTED_EDGE('',*,*,#4749,.F.);
#6738=ORIENTED_EDGE('',*,*,#4746,.F.);
#6739=ORIENTED_EDGE('',*,*,#4743,.F.);
#6740=ORIENTED_EDGE('',*,*,#4740,.F.);
#6741=ORIENTED_EDGE('',*,*,#4737,.F.);
#6742=ORIENTED_EDGE('',*,*,#4734,.F.);
#6743=ORIENTED_EDGE('',*,*,#4731,.F.);
#6744=ORIENTED_EDGE('',*,*,#4728,.F.);
#6745=ORIENTED_EDGE('',*,*,#4725,.F.);
#6746=ORIENTED_EDGE('',*,*,#4722,.F.);
#6747=ORIENTED_EDGE('',*,*,#4719,.F.);
#6748=ORIENTED_EDGE('',*,*,#4716,.F.);
#6749=ORIENTED_EDGE('',*,*,#4713,.F.);
#6750=ORIENTED_EDGE('',*,*,#4710,.F.);
#6751=ORIENTED_EDGE('',*,*,#4707,.F.);
#6752=ORIENTED_EDGE('',*,*,#4704,.F.);
#6753=ORIENTED_EDGE('',*,*,#4701,.F.);
#6754=ORIENTED_EDGE('',*,*,#4698,.F.);
#6755=ORIENTED_EDGE('',*,*,#4695,.F.);
#6756=ORIENTED_EDGE('',*,*,#4692,.F.);
#6757=ORIENTED_EDGE('',*,*,#4689,.F.);
#6758=ORIENTED_EDGE('',*,*,#4686,.F.);
#6759=ORIENTED_EDGE('',*,*,#4683,.F.);
#6760=ORIENTED_EDGE('',*,*,#4680,.F.);
#6761=ORIENTED_EDGE('',*,*,#4677,.F.);
#6762=ORIENTED_EDGE('',*,*,#4674,.F.);
#6763=ORIENTED_EDGE('',*,*,#4671,.F.);
#6764=ORIENTED_EDGE('',*,*,#4668,.F.);
#6765=ORIENTED_EDGE('',*,*,#4665,.F.);
#6766=ORIENTED_EDGE('',*,*,#4662,.F.);
#6767=ORIENTED_EDGE('',*,*,#4659,.F.);
#6768=ORIENTED_EDGE('',*,*,#4656,.F.);
#6769=ORIENTED_EDGE('',*,*,#4653,.F.);
#6770=ORIENTED_EDGE('',*,*,#4650,.F.);
#6771=ORIENTED_EDGE('',*,*,#4647,.F.);
#6772=ORIENTED_EDGE('',*,*,#4644,.F.);
#6773=ORIENTED_EDGE('',*,*,#4641,.F.);
#6774=ORIENTED_EDGE('',*,*,#4638,.F.);
#6775=ORIENTED_EDGE('',*,*,#4635,.F.);
#6776=ORIENTED_EDGE('',*,*,#4632,.F.);
#6777=ORIENTED_EDGE('',*,*,#4629,.F.);
#6778=ORIENTED_EDGE('',*,*,#4626,.F.);
#6779=ORIENTED_EDGE('',*,*,#4623,.F.);
#6780=ORIENTED_EDGE('',*,*,#4620,.F.);
#6781=ORIENTED_EDGE('',*,*,#4617,.F.);
#6782=ORIENTED_EDGE('',*,*,#4614,.F.);
#6783=ORIENTED_EDGE('',*,*,#4611,.F.);
#6784=ORIENTED_EDGE('',*,*,#4608,.F.);
#6785=ORIENTED_EDGE('',*,*,#4605,.F.);
#6786=ORIENTED_EDGE('',*,*,#4602,.F.);
#6787=ORIENTED_EDGE('',*,*,#4599,.F.);
#6788=ORIENTED_EDGE('',*,*,#4978,.F.);
#6789=ORIENTED_EDGE('',*,*,#4979,.T.);
#6790=ORIENTED_EDGE('',*,*,#4975,.T.);
#6791=ORIENTED_EDGE('',*,*,#4972,.T.);
#6792=ORIENTED_EDGE('',*,*,#4969,.T.);
#6793=ORIENTED_EDGE('',*,*,#4966,.T.);
#6794=ORIENTED_EDGE('',*,*,#4963,.T.);
#6795=ORIENTED_EDGE('',*,*,#4960,.T.);
#6796=ORIENTED_EDGE('',*,*,#4957,.T.);
#6797=ORIENTED_EDGE('',*,*,#4954,.T.);
#6798=ORIENTED_EDGE('',*,*,#4951,.T.);
#6799=ORIENTED_EDGE('',*,*,#4948,.T.);
#6800=ORIENTED_EDGE('',*,*,#4945,.T.);
#6801=ORIENTED_EDGE('',*,*,#4942,.T.);
#6802=ORIENTED_EDGE('',*,*,#4939,.T.);
#6803=ORIENTED_EDGE('',*,*,#4936,.T.);
#6804=ORIENTED_EDGE('',*,*,#4933,.T.);
#6805=ORIENTED_EDGE('',*,*,#4930,.T.);
#6806=ORIENTED_EDGE('',*,*,#4927,.T.);
#6807=ORIENTED_EDGE('',*,*,#4924,.T.);
#6808=ORIENTED_EDGE('',*,*,#4921,.T.);
#6809=ORIENTED_EDGE('',*,*,#4918,.T.);
#6810=ORIENTED_EDGE('',*,*,#4915,.T.);
#6811=ORIENTED_EDGE('',*,*,#4912,.T.);
#6812=ORIENTED_EDGE('',*,*,#4909,.T.);
#6813=ORIENTED_EDGE('',*,*,#4906,.T.);
#6814=ORIENTED_EDGE('',*,*,#4903,.T.);
#6815=ORIENTED_EDGE('',*,*,#4900,.T.);
#6816=ORIENTED_EDGE('',*,*,#4897,.T.);
#6817=ORIENTED_EDGE('',*,*,#4894,.T.);
#6818=ORIENTED_EDGE('',*,*,#4891,.T.);
#6819=ORIENTED_EDGE('',*,*,#4888,.T.);
#6820=ORIENTED_EDGE('',*,*,#4885,.T.);
#6821=ORIENTED_EDGE('',*,*,#4882,.T.);
#6822=ORIENTED_EDGE('',*,*,#4879,.T.);
#6823=ORIENTED_EDGE('',*,*,#4876,.T.);
#6824=ORIENTED_EDGE('',*,*,#4873,.T.);
#6825=ORIENTED_EDGE('',*,*,#4870,.T.);
#6826=ORIENTED_EDGE('',*,*,#4867,.T.);
#6827=ORIENTED_EDGE('',*,*,#4864,.T.);
#6828=ORIENTED_EDGE('',*,*,#4861,.T.);
#6829=ORIENTED_EDGE('',*,*,#4858,.T.);
#6830=ORIENTED_EDGE('',*,*,#4855,.T.);
#6831=ORIENTED_EDGE('',*,*,#4852,.T.);
#6832=ORIENTED_EDGE('',*,*,#4849,.T.);
#6833=ORIENTED_EDGE('',*,*,#4846,.T.);
#6834=ORIENTED_EDGE('',*,*,#4843,.T.);
#6835=ORIENTED_EDGE('',*,*,#4840,.T.);
#6836=ORIENTED_EDGE('',*,*,#4837,.T.);
#6837=ORIENTED_EDGE('',*,*,#4834,.T.);
#6838=ORIENTED_EDGE('',*,*,#4831,.T.);
#6839=ORIENTED_EDGE('',*,*,#4828,.T.);
#6840=ORIENTED_EDGE('',*,*,#4825,.T.);
#6841=ORIENTED_EDGE('',*,*,#4822,.T.);
#6842=ORIENTED_EDGE('',*,*,#4819,.T.);
#6843=ORIENTED_EDGE('',*,*,#4816,.T.);
#6844=ORIENTED_EDGE('',*,*,#4813,.T.);
#6845=ORIENTED_EDGE('',*,*,#4810,.T.);
#6846=ORIENTED_EDGE('',*,*,#4807,.T.);
#6847=ORIENTED_EDGE('',*,*,#4804,.T.);
#6848=ORIENTED_EDGE('',*,*,#4801,.T.);
#6849=ORIENTED_EDGE('',*,*,#4798,.T.);
#6850=ORIENTED_EDGE('',*,*,#4795,.T.);
#6851=ORIENTED_EDGE('',*,*,#4792,.T.);
#6852=ORIENTED_EDGE('',*,*,#4973,.T.);
#6853=ORIENTED_EDGE('',*,*,#4979,.F.);
#6854=ORIENTED_EDGE('',*,*,#4980,.F.);
#6855=ORIENTED_EDGE('',*,*,#4981,.T.);
#6856=ORIENTED_EDGE('',*,*,#4982,.F.);
#6857=ORIENTED_EDGE('',*,*,#4787,.F.);
#6858=ORIENTED_EDGE('',*,*,#4790,.F.);
#6859=ORIENTED_EDGE('',*,*,#4794,.F.);
#6860=ORIENTED_EDGE('',*,*,#4797,.F.);
#6861=ORIENTED_EDGE('',*,*,#4800,.F.);
#6862=ORIENTED_EDGE('',*,*,#4803,.F.);
#6863=ORIENTED_EDGE('',*,*,#4806,.F.);
#6864=ORIENTED_EDGE('',*,*,#4809,.F.);
#6865=ORIENTED_EDGE('',*,*,#4812,.F.);
#6866=ORIENTED_EDGE('',*,*,#4815,.F.);
#6867=ORIENTED_EDGE('',*,*,#4818,.F.);
#6868=ORIENTED_EDGE('',*,*,#4821,.F.);
#6869=ORIENTED_EDGE('',*,*,#4824,.F.);
#6870=ORIENTED_EDGE('',*,*,#4827,.F.);
#6871=ORIENTED_EDGE('',*,*,#4830,.F.);
#6872=ORIENTED_EDGE('',*,*,#4833,.F.);
#6873=ORIENTED_EDGE('',*,*,#4836,.F.);
#6874=ORIENTED_EDGE('',*,*,#4839,.F.);
#6875=ORIENTED_EDGE('',*,*,#4842,.F.);
#6876=ORIENTED_EDGE('',*,*,#4845,.F.);
#6877=ORIENTED_EDGE('',*,*,#4848,.F.);
#6878=ORIENTED_EDGE('',*,*,#4851,.F.);
#6879=ORIENTED_EDGE('',*,*,#4854,.F.);
#6880=ORIENTED_EDGE('',*,*,#4857,.F.);
#6881=ORIENTED_EDGE('',*,*,#4860,.F.);
#6882=ORIENTED_EDGE('',*,*,#4863,.F.);
#6883=ORIENTED_EDGE('',*,*,#4866,.F.);
#6884=ORIENTED_EDGE('',*,*,#4869,.F.);
#6885=ORIENTED_EDGE('',*,*,#4872,.F.);
#6886=ORIENTED_EDGE('',*,*,#4875,.F.);
#6887=ORIENTED_EDGE('',*,*,#4878,.F.);
#6888=ORIENTED_EDGE('',*,*,#4881,.F.);
#6889=ORIENTED_EDGE('',*,*,#4884,.F.);
#6890=ORIENTED_EDGE('',*,*,#4887,.F.);
#6891=ORIENTED_EDGE('',*,*,#4890,.F.);
#6892=ORIENTED_EDGE('',*,*,#4893,.F.);
#6893=ORIENTED_EDGE('',*,*,#4896,.F.);
#6894=ORIENTED_EDGE('',*,*,#4899,.F.);
#6895=ORIENTED_EDGE('',*,*,#4902,.F.);
#6896=ORIENTED_EDGE('',*,*,#4905,.F.);
#6897=ORIENTED_EDGE('',*,*,#4908,.F.);
#6898=ORIENTED_EDGE('',*,*,#4911,.F.);
#6899=ORIENTED_EDGE('',*,*,#4914,.F.);
#6900=ORIENTED_EDGE('',*,*,#4917,.F.);
#6901=ORIENTED_EDGE('',*,*,#4920,.F.);
#6902=ORIENTED_EDGE('',*,*,#4923,.F.);
#6903=ORIENTED_EDGE('',*,*,#4926,.F.);
#6904=ORIENTED_EDGE('',*,*,#4929,.F.);
#6905=ORIENTED_EDGE('',*,*,#4932,.F.);
#6906=ORIENTED_EDGE('',*,*,#4935,.F.);
#6907=ORIENTED_EDGE('',*,*,#4938,.F.);
#6908=ORIENTED_EDGE('',*,*,#4941,.F.);
#6909=ORIENTED_EDGE('',*,*,#4944,.F.);
#6910=ORIENTED_EDGE('',*,*,#4947,.F.);
#6911=ORIENTED_EDGE('',*,*,#4950,.F.);
#6912=ORIENTED_EDGE('',*,*,#4953,.F.);
#6913=ORIENTED_EDGE('',*,*,#4956,.F.);
#6914=ORIENTED_EDGE('',*,*,#4959,.F.);
#6915=ORIENTED_EDGE('',*,*,#4962,.F.);
#6916=ORIENTED_EDGE('',*,*,#4965,.F.);
#6917=ORIENTED_EDGE('',*,*,#4968,.F.);
#6918=ORIENTED_EDGE('',*,*,#4971,.F.);
#6919=ORIENTED_EDGE('',*,*,#4974,.F.);
#6920=ORIENTED_EDGE('',*,*,#4981,.F.);
#6921=ORIENTED_EDGE('',*,*,#4983,.F.);
#6922=ORIENTED_EDGE('',*,*,#4597,.F.);
#6923=ORIENTED_EDGE('',*,*,#4601,.F.);
#6924=ORIENTED_EDGE('',*,*,#4604,.F.);
#6925=ORIENTED_EDGE('',*,*,#4607,.F.);
#6926=ORIENTED_EDGE('',*,*,#4610,.F.);
#6927=ORIENTED_EDGE('',*,*,#4613,.F.);
#6928=ORIENTED_EDGE('',*,*,#4616,.F.);
#6929=ORIENTED_EDGE('',*,*,#4619,.F.);
#6930=ORIENTED_EDGE('',*,*,#4622,.F.);
#6931=ORIENTED_EDGE('',*,*,#4625,.F.);
#6932=ORIENTED_EDGE('',*,*,#4628,.F.);
#6933=ORIENTED_EDGE('',*,*,#4631,.F.);
#6934=ORIENTED_EDGE('',*,*,#4634,.F.);
#6935=ORIENTED_EDGE('',*,*,#4637,.F.);
#6936=ORIENTED_EDGE('',*,*,#4640,.F.);
#6937=ORIENTED_EDGE('',*,*,#4643,.F.);
#6938=ORIENTED_EDGE('',*,*,#4646,.F.);
#6939=ORIENTED_EDGE('',*,*,#4649,.F.);
#6940=ORIENTED_EDGE('',*,*,#4652,.F.);
#6941=ORIENTED_EDGE('',*,*,#4655,.F.);
#6942=ORIENTED_EDGE('',*,*,#4658,.F.);
#6943=ORIENTED_EDGE('',*,*,#4661,.F.);
#6944=ORIENTED_EDGE('',*,*,#4664,.F.);
#6945=ORIENTED_EDGE('',*,*,#4667,.F.);
#6946=ORIENTED_EDGE('',*,*,#4670,.F.);
#6947=ORIENTED_EDGE('',*,*,#4673,.F.);
#6948=ORIENTED_EDGE('',*,*,#4676,.F.);
#6949=ORIENTED_EDGE('',*,*,#4679,.F.);
#6950=ORIENTED_EDGE('',*,*,#4682,.F.);
#6951=ORIENTED_EDGE('',*,*,#4685,.F.);
#6952=ORIENTED_EDGE('',*,*,#4688,.F.);
#6953=ORIENTED_EDGE('',*,*,#4691,.F.);
#6954=ORIENTED_EDGE('',*,*,#4694,.F.);
#6955=ORIENTED_EDGE('',*,*,#4697,.F.);
#6956=ORIENTED_EDGE('',*,*,#4700,.F.);
#6957=ORIENTED_EDGE('',*,*,#4703,.F.);
#6958=ORIENTED_EDGE('',*,*,#4706,.F.);
#6959=ORIENTED_EDGE('',*,*,#4709,.F.);
#6960=ORIENTED_EDGE('',*,*,#4712,.F.);
#6961=ORIENTED_EDGE('',*,*,#4715,.F.);
#6962=ORIENTED_EDGE('',*,*,#4718,.F.);
#6963=ORIENTED_EDGE('',*,*,#4721,.F.);
#6964=ORIENTED_EDGE('',*,*,#4724,.F.);
#6965=ORIENTED_EDGE('',*,*,#4727,.F.);
#6966=ORIENTED_EDGE('',*,*,#4730,.F.);
#6967=ORIENTED_EDGE('',*,*,#4733,.F.);
#6968=ORIENTED_EDGE('',*,*,#4736,.F.);
#6969=ORIENTED_EDGE('',*,*,#4739,.F.);
#6970=ORIENTED_EDGE('',*,*,#4742,.F.);
#6971=ORIENTED_EDGE('',*,*,#4745,.F.);
#6972=ORIENTED_EDGE('',*,*,#4748,.F.);
#6973=ORIENTED_EDGE('',*,*,#4751,.F.);
#6974=ORIENTED_EDGE('',*,*,#4754,.F.);
#6975=ORIENTED_EDGE('',*,*,#4757,.F.);
#6976=ORIENTED_EDGE('',*,*,#4760,.F.);
#6977=ORIENTED_EDGE('',*,*,#4763,.F.);
#6978=ORIENTED_EDGE('',*,*,#4766,.F.);
#6979=ORIENTED_EDGE('',*,*,#4769,.F.);
#6980=ORIENTED_EDGE('',*,*,#4772,.F.);
#6981=ORIENTED_EDGE('',*,*,#4775,.F.);
#6982=ORIENTED_EDGE('',*,*,#4778,.F.);
#6983=ORIENTED_EDGE('',*,*,#4781,.F.);
#6984=ORIENTED_EDGE('',*,*,#4784,.F.);
#6985=ORIENTED_EDGE('',*,*,#4984,.F.);
#6986=ORIENTED_EDGE('',*,*,#4985,.F.);
#6987=ORIENTED_EDGE('',*,*,#4986,.T.);
#6988=ORIENTED_EDGE('',*,*,#4987,.F.);
#6989=ORIENTED_EDGE('',*,*,#4988,.F.);
#6990=ORIENTED_EDGE('',*,*,#4989,.F.);
#6991=ORIENTED_EDGE('',*,*,#4988,.T.);
#6992=ORIENTED_EDGE('',*,*,#4990,.T.);
#6993=ORIENTED_EDGE('',*,*,#4991,.T.);
#6994=ORIENTED_EDGE('',*,*,#4990,.F.);
#6995=ORIENTED_EDGE('',*,*,#4987,.T.);
#6996=ORIENTED_EDGE('',*,*,#4992,.T.);
#6997=ORIENTED_EDGE('',*,*,#4993,.F.);
#6998=ORIENTED_EDGE('',*,*,#4994,.F.);
#6999=ORIENTED_EDGE('',*,*,#4991,.F.);
#7000=ORIENTED_EDGE('',*,*,#4993,.T.);
#7001=ORIENTED_EDGE('',*,*,#4995,.T.);
#7002=ORIENTED_EDGE('',*,*,#4996,.F.);
#7003=ORIENTED_EDGE('',*,*,#4995,.F.);
#7004=ORIENTED_EDGE('',*,*,#4992,.F.);
#7005=ORIENTED_EDGE('',*,*,#4986,.F.);
#7006=ORIENTED_EDGE('',*,*,#4997,.F.);
#7007=ORIENTED_EDGE('',*,*,#4998,.T.);
#7008=ORIENTED_EDGE('',*,*,#4999,.F.);
#7009=ORIENTED_EDGE('',*,*,#4998,.F.);
#7010=ORIENTED_EDGE('',*,*,#4994,.T.);
#7011=ORIENTED_EDGE('',*,*,#4996,.T.);
#7012=ORIENTED_EDGE('',*,*,#4985,.T.);
#7013=ORIENTED_EDGE('',*,*,#4989,.T.);
#7014=ORIENTED_EDGE('',*,*,#4997,.T.);
#7015=ORIENTED_EDGE('',*,*,#5000,.F.);
#7016=ORIENTED_EDGE('',*,*,#5001,.T.);
#7017=ORIENTED_EDGE('',*,*,#4976,.T.);
#7018=ORIENTED_EDGE('',*,*,#4791,.T.);
#7019=ORIENTED_EDGE('',*,*,#4788,.T.);
#7020=ORIENTED_EDGE('',*,*,#4982,.T.);
#7021=ORIENTED_EDGE('',*,*,#5002,.F.);
#7022=ORIENTED_EDGE('',*,*,#5003,.T.);
#7023=ORIENTED_EDGE('',*,*,#5000,.T.);
#7024=ORIENTED_EDGE('',*,*,#5003,.F.);
#7025=ORIENTED_EDGE('',*,*,#5002,.T.);
#7026=ORIENTED_EDGE('',*,*,#4999,.T.);
#7027=ORIENTED_EDGE('',*,*,#4783,.T.);
#7028=ORIENTED_EDGE('',*,*,#4977,.T.);
#7029=ORIENTED_EDGE('',*,*,#5001,.F.);
#7030=ORIENTED_EDGE('',*,*,#4984,.T.);
#7031=ORIENTED_EDGE('',*,*,#4978,.T.);
#7032=ORIENTED_EDGE('',*,*,#4598,.F.);
#7033=ORIENTED_EDGE('',*,*,#4983,.T.);
#7034=ORIENTED_EDGE('',*,*,#4980,.T.);
#7035=ORIENTED_EDGE('',*,*,#5004,.F.);
#7036=ORIENTED_EDGE('',*,*,#5005,.T.);
#7037=ORIENTED_EDGE('',*,*,#5006,.T.);
#7038=ORIENTED_EDGE('',*,*,#5005,.F.);
#7039=ORIENTED_EDGE('',*,*,#5007,.F.);
#7040=ORIENTED_EDGE('',*,*,#5008,.T.);
#7041=ORIENTED_EDGE('',*,*,#5009,.T.);
#7042=ORIENTED_EDGE('',*,*,#5008,.F.);
#7043=ORIENTED_EDGE('',*,*,#5007,.T.);
#7044=ORIENTED_EDGE('',*,*,#5004,.T.);
#7045=ORIENTED_EDGE('',*,*,#5009,.F.);
#7046=ORIENTED_EDGE('',*,*,#5006,.F.);
#7047=ORIENTED_EDGE('',*,*,#5010,.F.);
#7048=ORIENTED_EDGE('',*,*,#5011,.T.);
#7049=ORIENTED_EDGE('',*,*,#5012,.F.);
#7050=ORIENTED_EDGE('',*,*,#5013,.F.);
#7051=ORIENTED_EDGE('',*,*,#5014,.F.);
#7052=ORIENTED_EDGE('',*,*,#5011,.F.);
#7053=ORIENTED_EDGE('',*,*,#5015,.F.);
#7054=ORIENTED_EDGE('',*,*,#5016,.T.);
#7055=ORIENTED_EDGE('',*,*,#5017,.F.);
#7056=ORIENTED_EDGE('',*,*,#5018,.F.);
#7057=ORIENTED_EDGE('',*,*,#5016,.F.);
#7058=ORIENTED_EDGE('',*,*,#5019,.F.);
#7059=ORIENTED_EDGE('',*,*,#5013,.T.);
#7060=ORIENTED_EDGE('',*,*,#5020,.F.);
#7061=ORIENTED_EDGE('',*,*,#5021,.T.);
#7062=ORIENTED_EDGE('',*,*,#5022,.T.);
#7063=ORIENTED_EDGE('',*,*,#5021,.F.);
#7064=ORIENTED_EDGE('',*,*,#5014,.T.);
#7065=ORIENTED_EDGE('',*,*,#5019,.T.);
#7066=ORIENTED_EDGE('',*,*,#5012,.T.);
#7067=ORIENTED_EDGE('',*,*,#5015,.T.);
#7068=ORIENTED_EDGE('',*,*,#5010,.T.);
#7069=ORIENTED_EDGE('',*,*,#5023,.F.);
#7070=ORIENTED_EDGE('',*,*,#5024,.T.);
#7071=ORIENTED_EDGE('',*,*,#5025,.T.);
#7072=ORIENTED_EDGE('',*,*,#5024,.F.);
#7073=ORIENTED_EDGE('',*,*,#5017,.T.);
#7074=ORIENTED_EDGE('',*,*,#5018,.T.);
#7075=ORIENTED_EDGE('',*,*,#5023,.T.);
#7076=ORIENTED_EDGE('',*,*,#5020,.T.);
#7077=ORIENTED_EDGE('',*,*,#5025,.F.);
#7078=ORIENTED_EDGE('',*,*,#5022,.F.);
#7079=ORIENTED_EDGE('',*,*,#5026,.F.);
#7080=ORIENTED_EDGE('',*,*,#5027,.T.);
#7081=ORIENTED_EDGE('',*,*,#5028,.F.);
#7082=ORIENTED_EDGE('',*,*,#5027,.F.);
#7083=ORIENTED_EDGE('',*,*,#5029,.F.);
#7084=ORIENTED_EDGE('',*,*,#5030,.T.);
#7085=ORIENTED_EDGE('',*,*,#5031,.F.);
#7086=ORIENTED_EDGE('',*,*,#5032,.F.);
#7087=ORIENTED_EDGE('',*,*,#5033,.F.);
#7088=ORIENTED_EDGE('',*,*,#5030,.F.);
#7089=ORIENTED_EDGE('',*,*,#5034,.F.);
#7090=ORIENTED_EDGE('',*,*,#5035,.T.);
#7091=ORIENTED_EDGE('',*,*,#5036,.F.);
#7092=ORIENTED_EDGE('',*,*,#5037,.F.);
#7093=ORIENTED_EDGE('',*,*,#5035,.F.);
#7094=ORIENTED_EDGE('',*,*,#5038,.F.);
#7095=ORIENTED_EDGE('',*,*,#5032,.T.);
#7096=ORIENTED_EDGE('',*,*,#5039,.F.);
#7097=ORIENTED_EDGE('',*,*,#5040,.F.);
#7098=ORIENTED_EDGE('',*,*,#5041,.F.);
#7099=ORIENTED_EDGE('',*,*,#5042,.F.);
#7100=ORIENTED_EDGE('',*,*,#5043,.F.);
#7101=ORIENTED_EDGE('',*,*,#5044,.F.);
#7102=ORIENTED_EDGE('',*,*,#5045,.F.);
#7103=ORIENTED_EDGE('',*,*,#5046,.F.);
#7104=ORIENTED_EDGE('',*,*,#5047,.F.);
#7105=ORIENTED_EDGE('',*,*,#5040,.T.);
#7106=ORIENTED_EDGE('',*,*,#5048,.F.);
#7107=ORIENTED_EDGE('',*,*,#5049,.F.);
#7108=ORIENTED_EDGE('',*,*,#5050,.F.);
#7109=ORIENTED_EDGE('',*,*,#5051,.F.);
#7110=ORIENTED_EDGE('',*,*,#5052,.F.);
#7111=ORIENTED_EDGE('',*,*,#5046,.T.);
#7112=ORIENTED_EDGE('',*,*,#5053,.T.);
#7113=ORIENTED_EDGE('',*,*,#5028,.T.);
#7114=ORIENTED_EDGE('',*,*,#5048,.T.);
#7115=ORIENTED_EDGE('',*,*,#5045,.T.);
#7116=ORIENTED_EDGE('',*,*,#5039,.T.);
#7117=ORIENTED_EDGE('',*,*,#5054,.T.);
#7118=ORIENTED_EDGE('',*,*,#5055,.F.);
#7119=ORIENTED_EDGE('',*,*,#5026,.T.);
#7120=ORIENTED_EDGE('',*,*,#5052,.T.);
#7121=ORIENTED_EDGE('',*,*,#5056,.T.);
#7122=ORIENTED_EDGE('',*,*,#5041,.T.);
#7123=ORIENTED_EDGE('',*,*,#5047,.T.);
#7124=ORIENTED_EDGE('',*,*,#5053,.F.);
#7125=ORIENTED_EDGE('',*,*,#5057,.T.);
#7126=ORIENTED_EDGE('',*,*,#5055,.T.);
#7127=ORIENTED_EDGE('',*,*,#5057,.F.);
#7128=ORIENTED_EDGE('',*,*,#5049,.T.);
#7129=ORIENTED_EDGE('',*,*,#5054,.F.);
#7130=ORIENTED_EDGE('',*,*,#5044,.T.);
#7131=ORIENTED_EDGE('',*,*,#5058,.T.);
#7132=ORIENTED_EDGE('',*,*,#5033,.T.);
#7133=ORIENTED_EDGE('',*,*,#5038,.T.);
#7134=ORIENTED_EDGE('',*,*,#5031,.T.);
#7135=ORIENTED_EDGE('',*,*,#5034,.T.);
#7136=ORIENTED_EDGE('',*,*,#5029,.T.);
#7137=ORIENTED_EDGE('',*,*,#5051,.T.);
#7138=ORIENTED_EDGE('',*,*,#5059,.T.);
#7139=ORIENTED_EDGE('',*,*,#5042,.T.);
#7140=ORIENTED_EDGE('',*,*,#5056,.F.);
#7141=ORIENTED_EDGE('',*,*,#5036,.T.);
#7142=ORIENTED_EDGE('',*,*,#5037,.T.);
#7143=ORIENTED_EDGE('',*,*,#5050,.T.);
#7144=ORIENTED_EDGE('',*,*,#5058,.F.);
#7145=ORIENTED_EDGE('',*,*,#5043,.T.);
#7146=ORIENTED_EDGE('',*,*,#5059,.F.);
#7147=ORIENTED_EDGE('',*,*,#5060,.F.);
#7148=ORIENTED_EDGE('',*,*,#5061,.T.);
#7149=ORIENTED_EDGE('',*,*,#5062,.T.);
#7150=ORIENTED_EDGE('',*,*,#5061,.F.);
#7151=ORIENTED_EDGE('',*,*,#5063,.F.);
#7152=ORIENTED_EDGE('',*,*,#5064,.T.);
#7153=ORIENTED_EDGE('',*,*,#5065,.T.);
#7154=ORIENTED_EDGE('',*,*,#5064,.F.);
#7155=ORIENTED_EDGE('',*,*,#5063,.T.);
#7156=ORIENTED_EDGE('',*,*,#5060,.T.);
#7157=ORIENTED_EDGE('',*,*,#5065,.F.);
#7158=ORIENTED_EDGE('',*,*,#5062,.F.);
#7159=ORIENTED_EDGE('',*,*,#5066,.F.);
#7160=ORIENTED_EDGE('',*,*,#5067,.T.);
#7161=ORIENTED_EDGE('',*,*,#5068,.T.);
#7162=ORIENTED_EDGE('',*,*,#5067,.F.);
#7163=ORIENTED_EDGE('',*,*,#5069,.F.);
#7164=ORIENTED_EDGE('',*,*,#5070,.T.);
#7165=ORIENTED_EDGE('',*,*,#5071,.T.);
#7166=ORIENTED_EDGE('',*,*,#5070,.F.);
#7167=ORIENTED_EDGE('',*,*,#5069,.T.);
#7168=ORIENTED_EDGE('',*,*,#5066,.T.);
#7169=ORIENTED_EDGE('',*,*,#5071,.F.);
#7170=ORIENTED_EDGE('',*,*,#5068,.F.);
#7171=ORIENTED_EDGE('',*,*,#5072,.F.);
#7172=ORIENTED_EDGE('',*,*,#5073,.F.);
#7173=ORIENTED_EDGE('',*,*,#5074,.F.);
#7174=ORIENTED_EDGE('',*,*,#5075,.F.);
#7175=ORIENTED_EDGE('',*,*,#5076,.F.);
#7176=ORIENTED_EDGE('',*,*,#5077,.F.);
#7177=ORIENTED_EDGE('',*,*,#5078,.F.);
#7178=ORIENTED_EDGE('',*,*,#5079,.F.);
#7179=ORIENTED_EDGE('',*,*,#5076,.T.);
#7180=ORIENTED_EDGE('',*,*,#5080,.T.);
#7181=ORIENTED_EDGE('',*,*,#5081,.T.);
#7182=ORIENTED_EDGE('',*,*,#5082,.T.);
#7183=ORIENTED_EDGE('',*,*,#5075,.T.);
#7184=ORIENTED_EDGE('',*,*,#5083,.F.);
#7185=ORIENTED_EDGE('',*,*,#5084,.T.);
#7186=ORIENTED_EDGE('',*,*,#5080,.F.);
#7187=ORIENTED_EDGE('',*,*,#5074,.T.);
#7188=ORIENTED_EDGE('',*,*,#5085,.T.);
#7189=ORIENTED_EDGE('',*,*,#5086,.T.);
#7190=ORIENTED_EDGE('',*,*,#5083,.T.);
#7191=ORIENTED_EDGE('',*,*,#5073,.T.);
#7192=ORIENTED_EDGE('',*,*,#5087,.F.);
#7193=ORIENTED_EDGE('',*,*,#5088,.T.);
#7194=ORIENTED_EDGE('',*,*,#5085,.F.);
#7195=ORIENTED_EDGE('',*,*,#5089,.F.);
#7196=ORIENTED_EDGE('',*,*,#5090,.F.);
#7197=ORIENTED_EDGE('',*,*,#5081,.F.);
#7198=ORIENTED_EDGE('',*,*,#5084,.F.);
#7199=ORIENTED_EDGE('',*,*,#5086,.F.);
#7200=ORIENTED_EDGE('',*,*,#5088,.F.);
#7201=ORIENTED_EDGE('',*,*,#5091,.F.);
#7202=ORIENTED_EDGE('',*,*,#5092,.F.);
#7203=ORIENTED_EDGE('',*,*,#5077,.T.);
#7204=ORIENTED_EDGE('',*,*,#5082,.F.);
#7205=ORIENTED_EDGE('',*,*,#5090,.T.);
#7206=ORIENTED_EDGE('',*,*,#5093,.F.);
#7207=ORIENTED_EDGE('',*,*,#5072,.T.);
#7208=ORIENTED_EDGE('',*,*,#5094,.T.);
#7209=ORIENTED_EDGE('',*,*,#5091,.T.);
#7210=ORIENTED_EDGE('',*,*,#5087,.T.);
#7211=ORIENTED_EDGE('',*,*,#5078,.T.);
#7212=ORIENTED_EDGE('',*,*,#5093,.T.);
#7213=ORIENTED_EDGE('',*,*,#5089,.T.);
#7214=ORIENTED_EDGE('',*,*,#5095,.T.);
#7215=ORIENTED_EDGE('',*,*,#5079,.T.);
#7216=ORIENTED_EDGE('',*,*,#5095,.F.);
#7217=ORIENTED_EDGE('',*,*,#5092,.T.);
#7218=ORIENTED_EDGE('',*,*,#5094,.F.);
#7219=ORIENTED_EDGE('',*,*,#5096,.F.);
#7220=ORIENTED_EDGE('',*,*,#5097,.T.);
#7221=ORIENTED_EDGE('',*,*,#5098,.T.);
#7222=ORIENTED_EDGE('',*,*,#5099,.F.);
#7223=ORIENTED_EDGE('',*,*,#5100,.F.);
#7224=ORIENTED_EDGE('',*,*,#5101,.T.);
#7225=ORIENTED_EDGE('',*,*,#5102,.T.);
#7226=ORIENTED_EDGE('',*,*,#5097,.F.);
#7227=ORIENTED_EDGE('',*,*,#5103,.F.);
#7228=ORIENTED_EDGE('',*,*,#5104,.T.);
#7229=ORIENTED_EDGE('',*,*,#5105,.T.);
#7230=ORIENTED_EDGE('',*,*,#5101,.F.);
#7231=ORIENTED_EDGE('',*,*,#5106,.F.);
#7232=ORIENTED_EDGE('',*,*,#5107,.T.);
#7233=ORIENTED_EDGE('',*,*,#5108,.T.);
#7234=ORIENTED_EDGE('',*,*,#5104,.F.);
#7235=ORIENTED_EDGE('',*,*,#5109,.F.);
#7236=ORIENTED_EDGE('',*,*,#5110,.T.);
#7237=ORIENTED_EDGE('',*,*,#5111,.T.);
#7238=ORIENTED_EDGE('',*,*,#5107,.F.);
#7239=ORIENTED_EDGE('',*,*,#5112,.F.);
#7240=ORIENTED_EDGE('',*,*,#5099,.T.);
#7241=ORIENTED_EDGE('',*,*,#5113,.T.);
#7242=ORIENTED_EDGE('',*,*,#5110,.F.);
#7243=ORIENTED_EDGE('',*,*,#5113,.F.);
#7244=ORIENTED_EDGE('',*,*,#5098,.F.);
#7245=ORIENTED_EDGE('',*,*,#5102,.F.);
#7246=ORIENTED_EDGE('',*,*,#5105,.F.);
#7247=ORIENTED_EDGE('',*,*,#5108,.F.);
#7248=ORIENTED_EDGE('',*,*,#5111,.F.);
#7249=ORIENTED_EDGE('',*,*,#5114,.F.);
#7250=ORIENTED_EDGE('',*,*,#5096,.T.);
#7251=ORIENTED_EDGE('',*,*,#5112,.T.);
#7252=ORIENTED_EDGE('',*,*,#5109,.T.);
#7253=ORIENTED_EDGE('',*,*,#5106,.T.);
#7254=ORIENTED_EDGE('',*,*,#5103,.T.);
#7255=ORIENTED_EDGE('',*,*,#5100,.T.);
#7256=ORIENTED_EDGE('',*,*,#5115,.F.);
#7257=ORIENTED_EDGE('',*,*,#5116,.T.);
#7258=ORIENTED_EDGE('',*,*,#5114,.T.);
#7259=ORIENTED_EDGE('',*,*,#5116,.F.);
#7260=ORIENTED_EDGE('',*,*,#5117,.F.);
#7261=ORIENTED_EDGE('',*,*,#5118,.T.);
#7262=ORIENTED_EDGE('',*,*,#5115,.T.);
#7263=ORIENTED_EDGE('',*,*,#5118,.F.);
#7264=ORIENTED_EDGE('',*,*,#5119,.F.);
#7265=ORIENTED_EDGE('',*,*,#5120,.T.);
#7266=ORIENTED_EDGE('',*,*,#5117,.T.);
#7267=ORIENTED_EDGE('',*,*,#5120,.F.);
#7268=ORIENTED_EDGE('',*,*,#5119,.T.);
#7269=ORIENTED_EDGE('',*,*,#5121,.F.);
#7270=ORIENTED_EDGE('',*,*,#5122,.T.);
#7271=ORIENTED_EDGE('',*,*,#5123,.T.);
#7272=ORIENTED_EDGE('',*,*,#5122,.F.);
#7273=ORIENTED_EDGE('',*,*,#5124,.F.);
#7274=ORIENTED_EDGE('',*,*,#5125,.T.);
#7275=ORIENTED_EDGE('',*,*,#5126,.T.);
#7276=ORIENTED_EDGE('',*,*,#5125,.F.);
#7277=ORIENTED_EDGE('',*,*,#5124,.T.);
#7278=ORIENTED_EDGE('',*,*,#5121,.T.);
#7279=ORIENTED_EDGE('',*,*,#5126,.F.);
#7280=ORIENTED_EDGE('',*,*,#5123,.F.);
#7281=ORIENTED_EDGE('',*,*,#5127,.F.);
#7282=ORIENTED_EDGE('',*,*,#5128,.F.);
#7283=ORIENTED_EDGE('',*,*,#5129,.T.);
#7284=ORIENTED_EDGE('',*,*,#5127,.T.);
#7285=ORIENTED_EDGE('',*,*,#5129,.F.);
#7286=ORIENTED_EDGE('',*,*,#5130,.F.);
#7287=ORIENTED_EDGE('',*,*,#5131,.T.);
#7288=ORIENTED_EDGE('',*,*,#5128,.T.);
#7289=ORIENTED_EDGE('',*,*,#5131,.F.);
#7290=ORIENTED_EDGE('',*,*,#5132,.F.);
#7291=ORIENTED_EDGE('',*,*,#5133,.T.);
#7292=ORIENTED_EDGE('',*,*,#5130,.T.);
#7293=ORIENTED_EDGE('',*,*,#5133,.F.);
#7294=ORIENTED_EDGE('',*,*,#5132,.T.);
#7295=ORIENTED_EDGE('',*,*,#5134,.F.);
#7296=ORIENTED_EDGE('',*,*,#5135,.F.);
#7297=ORIENTED_EDGE('',*,*,#5136,.T.);
#7298=ORIENTED_EDGE('',*,*,#5134,.T.);
#7299=ORIENTED_EDGE('',*,*,#5136,.F.);
#7300=ORIENTED_EDGE('',*,*,#5137,.F.);
#7301=ORIENTED_EDGE('',*,*,#5138,.T.);
#7302=ORIENTED_EDGE('',*,*,#5135,.T.);
#7303=ORIENTED_EDGE('',*,*,#5138,.F.);
#7304=ORIENTED_EDGE('',*,*,#5139,.F.);
#7305=ORIENTED_EDGE('',*,*,#5140,.T.);
#7306=ORIENTED_EDGE('',*,*,#5137,.T.);
#7307=ORIENTED_EDGE('',*,*,#5140,.F.);
#7308=ORIENTED_EDGE('',*,*,#5139,.T.);
#7309=ORIENTED_EDGE('',*,*,#5141,.T.);
#7310=ORIENTED_EDGE('',*,*,#5142,.T.);
#7311=ORIENTED_EDGE('',*,*,#5143,.T.);
#7312=ORIENTED_EDGE('',*,*,#5144,.F.);
#7313=ORIENTED_EDGE('',*,*,#5145,.T.);
#7314=ORIENTED_EDGE('',*,*,#5146,.T.);
#7315=ORIENTED_EDGE('',*,*,#5147,.T.);
#7316=ORIENTED_EDGE('',*,*,#5142,.F.);
#7317=ORIENTED_EDGE('',*,*,#5148,.T.);
#7318=ORIENTED_EDGE('',*,*,#5149,.T.);
#7319=ORIENTED_EDGE('',*,*,#5150,.T.);
#7320=ORIENTED_EDGE('',*,*,#5146,.F.);
#7321=ORIENTED_EDGE('',*,*,#5151,.T.);
#7322=ORIENTED_EDGE('',*,*,#5152,.T.);
#7323=ORIENTED_EDGE('',*,*,#5153,.T.);
#7324=ORIENTED_EDGE('',*,*,#5149,.F.);
#7325=ORIENTED_EDGE('',*,*,#5154,.T.);
#7326=ORIENTED_EDGE('',*,*,#5155,.T.);
#7327=ORIENTED_EDGE('',*,*,#5156,.T.);
#7328=ORIENTED_EDGE('',*,*,#5152,.F.);
#7329=ORIENTED_EDGE('',*,*,#5157,.T.);
#7330=ORIENTED_EDGE('',*,*,#5144,.T.);
#7331=ORIENTED_EDGE('',*,*,#5158,.T.);
#7332=ORIENTED_EDGE('',*,*,#5155,.F.);
#7333=ORIENTED_EDGE('',*,*,#5157,.F.);
#7334=ORIENTED_EDGE('',*,*,#5154,.F.);
#7335=ORIENTED_EDGE('',*,*,#5151,.F.);
#7336=ORIENTED_EDGE('',*,*,#5148,.F.);
#7337=ORIENTED_EDGE('',*,*,#5145,.F.);
#7338=ORIENTED_EDGE('',*,*,#5141,.F.);
#7339=ORIENTED_EDGE('',*,*,#5158,.F.);
#7340=ORIENTED_EDGE('',*,*,#5143,.F.);
#7341=ORIENTED_EDGE('',*,*,#5147,.F.);
#7342=ORIENTED_EDGE('',*,*,#5150,.F.);
#7343=ORIENTED_EDGE('',*,*,#5153,.F.);
#7344=ORIENTED_EDGE('',*,*,#5156,.F.);
#7345=CYLINDRICAL_SURFACE('',#8404,0.33);
#7346=CYLINDRICAL_SURFACE('',#8407,0.33);
#7347=CYLINDRICAL_SURFACE('',#8410,0.329999999999998);
#7348=CYLINDRICAL_SURFACE('',#8413,0.33);
#7349=CYLINDRICAL_SURFACE('',#8416,0.329999999999998);
#7350=CYLINDRICAL_SURFACE('',#8419,0.33);
#7351=CYLINDRICAL_SURFACE('',#8422,0.329999999999998);
#7352=CYLINDRICAL_SURFACE('',#8432,0.25);
#7353=CYLINDRICAL_SURFACE('',#8436,0.25);
#7354=CYLINDRICAL_SURFACE('',#8440,0.25);
#7355=CYLINDRICAL_SURFACE('',#8451,0.21);
#7356=CYLINDRICAL_SURFACE('',#8455,0.21);
#7357=CYLINDRICAL_SURFACE('',#8459,0.25);
#7358=CYLINDRICAL_SURFACE('',#8463,0.25);
#7359=CYLINDRICAL_SURFACE('',#8474,0.165);
#7360=CYLINDRICAL_SURFACE('',#8477,0.165);
#7361=CYLINDRICAL_SURFACE('',#8480,0.165);
#7362=CYLINDRICAL_SURFACE('',#8483,2.35);
#7363=CYLINDRICAL_SURFACE('',#8488,2.15);
#7364=CYLINDRICAL_SURFACE('',#8490,0.25);
#7365=CYLINDRICAL_SURFACE('',#8494,0.25);
#7366=CYLINDRICAL_SURFACE('',#8505,0.225);
#7367=CYLINDRICAL_SURFACE('',#8508,0.225);
#7368=CYLINDRICAL_SURFACE('',#8511,0.225);
#7369=CYLINDRICAL_SURFACE('',#8518,3.);
#7370=CYLINDRICAL_SURFACE('',#8520,2.34);
#7371=CYLINDRICAL_SURFACE('',#8524,1.8);
#7372=CYLINDRICAL_SURFACE('',#8537,0.475);
#7373=CYLINDRICAL_SURFACE('',#8541,0.475);
#7374=CYLINDRICAL_SURFACE('',#8545,0.275);
#7375=CYLINDRICAL_SURFACE('',#8546,0.275);
#7376=CYLINDRICAL_SURFACE('',#8563,0.5);
#7377=CYLINDRICAL_SURFACE('',#8571,0.2942);
#7378=CYLINDRICAL_SURFACE('',#8580,1.63531);
#7379=CYLINDRICAL_SURFACE('',#8582,1.);
#7380=CYLINDRICAL_SURFACE('',#8588,1.63531);
#7381=CYLINDRICAL_SURFACE('',#8600,1.71469);
#7382=CYLINDRICAL_SURFACE('',#8607,2.35);
#7383=CYLINDRICAL_SURFACE('',#8612,1.71469);
#7384=CYLINDRICAL_SURFACE('',#8634,1.706752);
#7385=CYLINDRICAL_SURFACE('',#8674,1.643248);
#7386=CYLINDRICAL_SURFACE('',#8688,1.70469);
#7387=CYLINDRICAL_SURFACE('',#8692,1.65031);
#7388=CYLINDRICAL_SURFACE('',#8696,1.70469);
#7389=CYLINDRICAL_SURFACE('',#8700,1.65031);
#7390=CYLINDRICAL_SURFACE('',#8708,0.165);
#7391=CYLINDRICAL_SURFACE('',#8712,0.165);
#7392=CYLINDRICAL_SURFACE('',#8716,0.165);
#7393=CYLINDRICAL_SURFACE('',#8720,0.21);
#7394=CYLINDRICAL_SURFACE('',#8724,0.21);
#7395=CYLINDRICAL_SURFACE('',#8728,0.475);
#7396=CYLINDRICAL_SURFACE('',#8733,0.210000000000001);
#7397=CYLINDRICAL_SURFACE('',#8735,0.475);
#7398=CYLINDRICAL_SURFACE('',#8740,0.210000000000001);
#7399=CYLINDRICAL_SURFACE('',#8742,1.11);
#7400=CYLINDRICAL_SURFACE('',#8772,0.475);
#7401=CYLINDRICAL_SURFACE('',#8776,0.475);
#7402=CYLINDRICAL_SURFACE('',#8780,0.275);
#7403=CYLINDRICAL_SURFACE('',#8781,0.275);
#7404=CYLINDRICAL_SURFACE('',#8784,0.457875);
#7405=CYLINDRICAL_SURFACE('',#8786,0.457875);
#7406=CYLINDRICAL_SURFACE('',#8787,0.457875);
#7407=CYLINDRICAL_SURFACE('',#8788,0.457875);
#7408=CYLINDRICAL_SURFACE('',#8789,0.457875);
#7409=CYLINDRICAL_SURFACE('',#8790,0.457875);
#7410=CYLINDRICAL_SURFACE('',#8791,0.457875);
#7411=CYLINDRICAL_SURFACE('',#8792,0.457875);
#7412=CYLINDRICAL_SURFACE('',#8793,0.457875);
#7413=CYLINDRICAL_SURFACE('',#8795,0.625);
#7414=CYLINDRICAL_SURFACE('',#8797,0.625);
#7415=CYLINDRICAL_SURFACE('',#8798,0.625);
#7416=CYLINDRICAL_SURFACE('',#8799,0.625);
#7417=CYLINDRICAL_SURFACE('',#8800,0.625);
#7418=CYLINDRICAL_SURFACE('',#8801,0.625);
#7419=CYLINDRICAL_SURFACE('',#8802,0.625);
#7420=CYLINDRICAL_SURFACE('',#8803,0.625);
#7421=CYLINDRICAL_SURFACE('',#8804,0.625);
#7422=CYLINDRICAL_SURFACE('',#8806,0.625);
#7423=CYLINDRICAL_SURFACE('',#8813,0.225);
#7424=CYLINDRICAL_SURFACE('',#8815,0.225);
#7425=CYLINDRICAL_SURFACE('',#8817,0.225);
#7426=CYLINDRICAL_SURFACE('',#8823,1.9);
#7427=CYLINDRICAL_SURFACE('',#8824,0.457875);
#7428=CYLINDRICAL_SURFACE('',#8825,1.1);
#7429=CYLINDRICAL_SURFACE('',#8833,0.425);
#7430=CYLINDRICAL_SURFACE('',#8841,0.24505);
#7431=CYLINDRICAL_SURFACE('',#8859,0.35);
#7432=CYLINDRICAL_SURFACE('',#8867,0.1954);
#7433=CYLINDRICAL_SURFACE('',#8893,0.5941);
#7434=CYLINDRICAL_SURFACE('',#8895,0.5941);
#7435=CYLINDRICAL_SURFACE('',#8896,0.5941);
#7436=CYLINDRICAL_SURFACE('',#8897,0.5941);
#7437=CYLINDRICAL_SURFACE('',#8898,0.5941);
#7438=CYLINDRICAL_SURFACE('',#8899,0.5941);
#7439=CYLINDRICAL_SURFACE('',#8900,0.5941);
#7440=CYLINDRICAL_SURFACE('',#8901,0.5941);
#7441=CYLINDRICAL_SURFACE('',#8902,0.5941);
#7442=CYLINDRICAL_SURFACE('',#8903,0.5941);
#7443=CYLINDRICAL_SURFACE('',#8904,0.5941);
#7444=CYLINDRICAL_SURFACE('',#8905,0.5941);
#7445=CYLINDRICAL_SURFACE('',#8906,0.5941);
#7446=CYLINDRICAL_SURFACE('',#8907,0.5941);
#7447=CYLINDRICAL_SURFACE('',#8908,0.5941);
#7448=CYLINDRICAL_SURFACE('',#8909,0.5941);
#7449=CYLINDRICAL_SURFACE('',#8910,0.5941);
#7450=CYLINDRICAL_SURFACE('',#8911,0.5941);
#7451=CYLINDRICAL_SURFACE('',#8912,0.5941);
#7452=CYLINDRICAL_SURFACE('',#8913,0.5941);
#7453=CYLINDRICAL_SURFACE('',#8914,0.5941);
#7454=CYLINDRICAL_SURFACE('',#8915,0.5941);
#7455=CYLINDRICAL_SURFACE('',#8916,0.5941);
#7456=CYLINDRICAL_SURFACE('',#8917,0.5941);
#7457=CYLINDRICAL_SURFACE('',#8918,0.5941);
#7458=CYLINDRICAL_SURFACE('',#8919,0.5941);
#7459=CYLINDRICAL_SURFACE('',#8920,0.5941);
#7460=CYLINDRICAL_SURFACE('',#8921,0.5941);
#7461=CYLINDRICAL_SURFACE('',#8922,0.5941);
#7462=CYLINDRICAL_SURFACE('',#8923,0.5941);
#7463=CYLINDRICAL_SURFACE('',#8924,0.5941);
#7464=CYLINDRICAL_SURFACE('',#8925,0.5941);
#7465=CYLINDRICAL_SURFACE('',#8926,0.5941);
#7466=CYLINDRICAL_SURFACE('',#8927,0.5941);
#7467=CYLINDRICAL_SURFACE('',#8928,0.5941);
#7468=CYLINDRICAL_SURFACE('',#8929,0.5941);
#7469=CYLINDRICAL_SURFACE('',#8930,0.5941);
#7470=CYLINDRICAL_SURFACE('',#8931,0.5941);
#7471=CYLINDRICAL_SURFACE('',#8932,0.5941);
#7472=CYLINDRICAL_SURFACE('',#8933,0.5941);
#7473=CYLINDRICAL_SURFACE('',#8934,0.5941);
#7474=CYLINDRICAL_SURFACE('',#8935,0.5941);
#7475=CYLINDRICAL_SURFACE('',#8936,0.5941);
#7476=CYLINDRICAL_SURFACE('',#8937,0.5941);
#7477=CYLINDRICAL_SURFACE('',#8938,0.5941);
#7478=CYLINDRICAL_SURFACE('',#8939,0.5941);
#7479=CYLINDRICAL_SURFACE('',#8940,0.5941);
#7480=CYLINDRICAL_SURFACE('',#8941,0.5941);
#7481=CYLINDRICAL_SURFACE('',#8942,0.5941);
#7482=CYLINDRICAL_SURFACE('',#8943,0.5941);
#7483=CYLINDRICAL_SURFACE('',#8944,0.5941);
#7484=CYLINDRICAL_SURFACE('',#8945,0.5941);
#7485=CYLINDRICAL_SURFACE('',#8946,0.5941);
#7486=CYLINDRICAL_SURFACE('',#8947,0.5941);
#7487=CYLINDRICAL_SURFACE('',#8948,0.5941);
#7488=CYLINDRICAL_SURFACE('',#8949,0.5941);
#7489=CYLINDRICAL_SURFACE('',#8950,0.5941);
#7490=CYLINDRICAL_SURFACE('',#8951,0.5941);
#7491=CYLINDRICAL_SURFACE('',#8952,0.5941);
#7492=CYLINDRICAL_SURFACE('',#8953,0.5941);
#7493=CYLINDRICAL_SURFACE('',#8954,0.5941);
#7494=CYLINDRICAL_SURFACE('',#8955,0.5941);
#7495=CYLINDRICAL_SURFACE('',#8956,0.5941);
#7496=CYLINDRICAL_SURFACE('',#8957,0.415875);
#7497=CYLINDRICAL_SURFACE('',#8959,0.415875);
#7498=CYLINDRICAL_SURFACE('',#8961,0.415875);
#7499=CYLINDRICAL_SURFACE('',#8962,0.415875);
#7500=CYLINDRICAL_SURFACE('',#8963,0.415875);
#7501=CYLINDRICAL_SURFACE('',#8964,0.415875);
#7502=CYLINDRICAL_SURFACE('',#8965,0.415875);
#7503=CYLINDRICAL_SURFACE('',#8966,0.415875);
#7504=CYLINDRICAL_SURFACE('',#8967,0.415875);
#7505=CYLINDRICAL_SURFACE('',#8968,0.415875);
#7506=CYLINDRICAL_SURFACE('',#8969,0.415875);
#7507=CYLINDRICAL_SURFACE('',#8970,0.415875);
#7508=CYLINDRICAL_SURFACE('',#8971,0.415875);
#7509=CYLINDRICAL_SURFACE('',#8972,0.415875);
#7510=CYLINDRICAL_SURFACE('',#8973,0.415875);
#7511=CYLINDRICAL_SURFACE('',#8974,0.415875);
#7512=CYLINDRICAL_SURFACE('',#8975,0.415875);
#7513=CYLINDRICAL_SURFACE('',#8976,0.415875);
#7514=CYLINDRICAL_SURFACE('',#8977,0.415875);
#7515=CYLINDRICAL_SURFACE('',#8978,0.415875);
#7516=CYLINDRICAL_SURFACE('',#8979,0.415875);
#7517=CYLINDRICAL_SURFACE('',#8980,0.415875);
#7518=CYLINDRICAL_SURFACE('',#8981,0.415875);
#7519=CYLINDRICAL_SURFACE('',#8982,0.415875);
#7520=CYLINDRICAL_SURFACE('',#8983,0.415875);
#7521=CYLINDRICAL_SURFACE('',#8984,0.415875);
#7522=CYLINDRICAL_SURFACE('',#8985,0.415875);
#7523=CYLINDRICAL_SURFACE('',#8986,0.415875);
#7524=CYLINDRICAL_SURFACE('',#8987,0.415875);
#7525=CYLINDRICAL_SURFACE('',#8988,0.415875);
#7526=CYLINDRICAL_SURFACE('',#8989,0.415875);
#7527=CYLINDRICAL_SURFACE('',#8990,0.415875);
#7528=CYLINDRICAL_SURFACE('',#8991,0.415875);
#7529=CYLINDRICAL_SURFACE('',#8992,0.415875);
#7530=CYLINDRICAL_SURFACE('',#8993,0.415875);
#7531=CYLINDRICAL_SURFACE('',#8994,0.415875);
#7532=CYLINDRICAL_SURFACE('',#8995,0.415875);
#7533=CYLINDRICAL_SURFACE('',#8996,0.415875);
#7534=CYLINDRICAL_SURFACE('',#8997,0.415875);
#7535=CYLINDRICAL_SURFACE('',#8998,0.415875);
#7536=CYLINDRICAL_SURFACE('',#8999,0.415875);
#7537=CYLINDRICAL_SURFACE('',#9000,0.415875);
#7538=CYLINDRICAL_SURFACE('',#9001,0.415875);
#7539=CYLINDRICAL_SURFACE('',#9002,0.415875);
#7540=CYLINDRICAL_SURFACE('',#9003,0.415875);
#7541=CYLINDRICAL_SURFACE('',#9004,0.415875);
#7542=CYLINDRICAL_SURFACE('',#9005,0.415875);
#7543=CYLINDRICAL_SURFACE('',#9006,0.415875);
#7544=CYLINDRICAL_SURFACE('',#9007,0.415875);
#7545=CYLINDRICAL_SURFACE('',#9008,0.415875);
#7546=CYLINDRICAL_SURFACE('',#9009,0.415875);
#7547=CYLINDRICAL_SURFACE('',#9010,0.415875);
#7548=CYLINDRICAL_SURFACE('',#9011,0.415875);
#7549=CYLINDRICAL_SURFACE('',#9012,0.415875);
#7550=CYLINDRICAL_SURFACE('',#9013,0.415875);
#7551=CYLINDRICAL_SURFACE('',#9014,0.415875);
#7552=CYLINDRICAL_SURFACE('',#9015,0.415875);
#7553=CYLINDRICAL_SURFACE('',#9016,0.415875);
#7554=CYLINDRICAL_SURFACE('',#9017,0.415875);
#7555=CYLINDRICAL_SURFACE('',#9018,0.415875);
#7556=CYLINDRICAL_SURFACE('',#9019,0.415875);
#7557=CYLINDRICAL_SURFACE('',#9020,0.415875);
#7558=CYLINDRICAL_SURFACE('',#9021,0.415875);
#7559=CYLINDRICAL_SURFACE('',#9022,0.415875);
#7560=CYLINDRICAL_SURFACE('',#9031,1.);
#7561=CYLINDRICAL_SURFACE('',#9038,1.35);
#7562=CYLINDRICAL_SURFACE('',#9041,0.5941);
#7563=CYLINDRICAL_SURFACE('',#9044,1.01);
#7564=CYLINDRICAL_SURFACE('',#9047,1.35);
#7565=CYLINDRICAL_SURFACE('',#9055,0.210000000000001);
#7566=CYLINDRICAL_SURFACE('',#9058,1.005);
#7567=CYLINDRICAL_SURFACE('',#9061,1.5);
#7568=CYLINDRICAL_SURFACE('',#9067,0.25);
#7569=CYLINDRICAL_SURFACE('',#9072,0.210000000000001);
#7570=CYLINDRICAL_SURFACE('',#9084,3.5);
#7571=CYLINDRICAL_SURFACE('',#9085,1.);
#7572=CYLINDRICAL_SURFACE('',#9087,1.5);
#7573=CYLINDRICAL_SURFACE('',#9091,0.33);
#7574=CYLINDRICAL_SURFACE('',#9094,0.4);
#7575=CYLINDRICAL_SURFACE('',#9100,0.405);
#7576=CYLINDRICAL_SURFACE('',#9103,0.9);
#7577=CYLINDRICAL_SURFACE('',#9131,0.24505);
#7578=CYLINDRICAL_SURFACE('',#9137,0.32);
#7579=CYLINDRICAL_SURFACE('',#9140,0.6);
#7580=CYLINDRICAL_SURFACE('',#9150,0.5);
#7581=CYLINDRICAL_SURFACE('',#9158,0.2942);
#7582=ADVANCED_FACE('',(#1012),#7345,.F.);
#7583=ADVANCED_FACE('',(#1013),#7346,.F.);
#7584=ADVANCED_FACE('',(#1014),#7347,.F.);
#7585=ADVANCED_FACE('',(#1015),#7348,.F.);
#7586=ADVANCED_FACE('',(#1016),#7349,.F.);
#7587=ADVANCED_FACE('',(#1017),#7350,.F.);
#7588=ADVANCED_FACE('',(#1018),#7351,.F.);
#7589=ADVANCED_FACE('',(#1019),#822,.T.);
#7590=ADVANCED_FACE('',(#1020),#823,.T.);
#7591=ADVANCED_FACE('',(#1021),#824,.T.);
#7592=ADVANCED_FACE('',(#1022),#825,.T.);
#7593=ADVANCED_FACE('',(#1023,#712,#713,#714,#715,#716,#717,#718),#826,
 .T.);
#7594=ADVANCED_FACE('',(#1024,#719,#720,#721,#722,#723,#724,#725),#827,
 .F.);
#7595=ADVANCED_FACE('',(#1025),#7352,.F.);
#7596=ADVANCED_FACE('',(#1026),#828,.F.);
#7597=ADVANCED_FACE('',(#1027),#7353,.F.);
#7598=ADVANCED_FACE('',(#1028),#829,.F.);
#7599=ADVANCED_FACE('',(#1029),#7354,.F.);
#7600=ADVANCED_FACE('',(#1030),#830,.F.);
#7601=ADVANCED_FACE('',(#1031),#831,.T.);
#7602=ADVANCED_FACE('',(#1032),#832,.T.);
#7603=ADVANCED_FACE('',(#1033,#726,#727,#728),#833,.T.);
#7604=ADVANCED_FACE('',(#1034),#834,.T.);
#7605=ADVANCED_FACE('',(#1035),#835,.T.);
#7606=ADVANCED_FACE('',(#1036),#836,.F.);
#7607=ADVANCED_FACE('',(#1037),#7355,.F.);
#7608=ADVANCED_FACE('',(#1038),#837,.T.);
#7609=ADVANCED_FACE('',(#1039),#7356,.F.);
#7610=ADVANCED_FACE('',(#1040),#838,.T.);
#7611=ADVANCED_FACE('',(#1041),#7357,.F.);
#7612=ADVANCED_FACE('',(#1042),#839,.F.);
#7613=ADVANCED_FACE('',(#1043),#7358,.F.);
#7614=ADVANCED_FACE('',(#1044),#840,.F.);
#7615=ADVANCED_FACE('',(#1045),#841,.T.);
#7616=ADVANCED_FACE('',(#1046,#729,#730),#842,.T.);
#7617=ADVANCED_FACE('',(#1047),#843,.T.);
#7618=ADVANCED_FACE('',(#1048),#844,.T.);
#7619=ADVANCED_FACE('',(#1049),#845,.T.);
#7620=ADVANCED_FACE('',(#1050,#731,#732),#846,.F.);
#7621=ADVANCED_FACE('',(#1051),#7359,.F.);
#7622=ADVANCED_FACE('',(#1052),#7360,.F.);
#7623=ADVANCED_FACE('',(#1053),#7361,.F.);
#7624=ADVANCED_FACE('',(#1054),#7362,.F.);
#7625=ADVANCED_FACE('',(#1055,#733),#847,.T.);
#7626=ADVANCED_FACE('',(#1056),#7363,.F.);
#7627=ADVANCED_FACE('',(#1057),#7364,.F.);
#7628=ADVANCED_FACE('',(#1058),#848,.F.);
#7629=ADVANCED_FACE('',(#1059),#7365,.F.);
#7630=ADVANCED_FACE('',(#1060),#849,.F.);
#7631=ADVANCED_FACE('',(#1061),#850,.T.);
#7632=ADVANCED_FACE('',(#1062,#734,#735,#736,#737),#851,.T.);
#7633=ADVANCED_FACE('',(#1063),#852,.T.);
#7634=ADVANCED_FACE('',(#1064,#738,#739,#740,#741),#853,.T.);
#7635=ADVANCED_FACE('',(#1065),#854,.T.);
#7636=ADVANCED_FACE('',(#1066,#742,#743),#855,.F.);
#7637=ADVANCED_FACE('',(#1067),#7366,.F.);
#7638=ADVANCED_FACE('',(#1068),#7367,.F.);
#7639=ADVANCED_FACE('',(#1069),#7368,.F.);
#7640=ADVANCED_FACE('',(#1070),#856,.F.);
#7641=ADVANCED_FACE('',(#1071,#744,#745,#746,#747),#857,.F.);
#7642=ADVANCED_FACE('',(#1072),#7369,.T.);
#7643=ADVANCED_FACE('',(#1073),#7370,.T.);
#7644=ADVANCED_FACE('',(#1074,#748),#858,.F.);
#7645=ADVANCED_FACE('',(#1075),#7371,.F.);
#7646=ADVANCED_FACE('',(#1076,#749,#750,#751,#752),#859,.T.);
#7647=ADVANCED_FACE('',(#1077),#860,.T.);
#7648=ADVANCED_FACE('',(#1078,#753,#754),#861,.T.);
#7649=ADVANCED_FACE('',(#1079),#862,.F.);
#7650=ADVANCED_FACE('',(#1080),#863,.F.);
#7651=ADVANCED_FACE('',(#1081,#755,#756),#864,.T.);
#7652=ADVANCED_FACE('',(#1082),#7372,.F.);
#7653=ADVANCED_FACE('',(#1083,#757),#865,.T.);
#7654=ADVANCED_FACE('',(#1084),#7373,.F.);
#7655=ADVANCED_FACE('',(#1085,#758),#866,.T.);
#7656=ADVANCED_FACE('',(#1086),#7374,.F.);
#7657=ADVANCED_FACE('',(#1087),#7375,.F.);
#7658=ADVANCED_FACE('',(#1088),#867,.T.);
#7659=ADVANCED_FACE('',(#1089),#868,.F.);
#7660=ADVANCED_FACE('',(#1090),#869,.F.);
#7661=ADVANCED_FACE('',(#1091),#870,.F.);
#7662=ADVANCED_FACE('',(#1092),#871,.F.);
#7663=ADVANCED_FACE('',(#1093),#872,.F.);
#7664=ADVANCED_FACE('',(#1094),#873,.F.);
#7665=ADVANCED_FACE('',(#1095),#874,.F.);
#7666=ADVANCED_FACE('',(#1096),#875,.F.);
#7667=ADVANCED_FACE('',(#1097),#876,.F.);
#7668=ADVANCED_FACE('',(#1098),#877,.T.);
#7669=ADVANCED_FACE('',(#1099),#559,.T.);
#7670=ADVANCED_FACE('',(#1100),#7376,.T.);
#7671=ADVANCED_FACE('',(#1101),#560,.T.);
#7672=ADVANCED_FACE('',(#1102,#759),#878,.T.);
#7673=ADVANCED_FACE('',(#1103),#561,.T.);
#7674=ADVANCED_FACE('',(#1104),#7377,.T.);
#7675=ADVANCED_FACE('',(#1105),#557,.F.);
#7676=ADVANCED_FACE('',(#1106),#7378,.T.);
#7677=ADVANCED_FACE('',(#1107),#7379,.F.);
#7678=ADVANCED_FACE('',(#1108),#562,.F.);
#7679=ADVANCED_FACE('',(#1109,#760),#879,.T.);
#7680=ADVANCED_FACE('',(#1110),#7380,.T.);
#7681=ADVANCED_FACE('',(#1111,#761),#880,.T.);
#7682=ADVANCED_FACE('',(#1112),#563,.F.);
#7683=ADVANCED_FACE('',(#1113),#558,.F.);
#7684=ADVANCED_FACE('',(#1114),#7381,.F.);
#7685=ADVANCED_FACE('',(#1115,#762),#881,.T.);
#7686=ADVANCED_FACE('',(#1116),#564,.T.);
#7687=ADVANCED_FACE('',(#1117),#7382,.T.);
#7688=ADVANCED_FACE('',(#1118),#565,.T.);
#7689=ADVANCED_FACE('',(#1119,#763),#882,.T.);
#7690=ADVANCED_FACE('',(#1120),#7383,.F.);
#7691=ADVANCED_FACE('',(#1121),#541,.T.);
#7692=ADVANCED_FACE('',(#1122),#542,.T.);
#7693=ADVANCED_FACE('',(#1123),#543,.T.);
#7694=ADVANCED_FACE('',(#1124),#544,.T.);
#7695=ADVANCED_FACE('',(#1125),#545,.T.);
#7696=ADVANCED_FACE('',(#1126),#546,.T.);
#7697=ADVANCED_FACE('',(#1127),#547,.T.);
#7698=ADVANCED_FACE('',(#1128),#548,.T.);
#7699=ADVANCED_FACE('',(#1129),#549,.F.);
#7700=ADVANCED_FACE('',(#1130),#7384,.T.);
#7701=ADVANCED_FACE('',(#1131),#883,.T.);
#7702=ADVANCED_FACE('',(#1132),#550,.F.);
#7703=ADVANCED_FACE('',(#1133),#884,.T.);
#7704=ADVANCED_FACE('',(#1134),#551,.F.);
#7705=ADVANCED_FACE('',(#1135),#885,.T.);
#7706=ADVANCED_FACE('',(#1136),#552,.F.);
#7707=ADVANCED_FACE('',(#1137),#886,.T.);
#7708=ADVANCED_FACE('',(#1138),#553,.F.);
#7709=ADVANCED_FACE('',(#1139),#887,.T.);
#7710=ADVANCED_FACE('',(#1140),#554,.F.);
#7711=ADVANCED_FACE('',(#1141),#888,.T.);
#7712=ADVANCED_FACE('',(#1142),#555,.F.);
#7713=ADVANCED_FACE('',(#1143),#7385,.F.);
#7714=ADVANCED_FACE('',(#1144),#889,.T.);
#7715=ADVANCED_FACE('',(#1145),#556,.F.);
#7716=ADVANCED_FACE('',(#1146,#764),#890,.T.);
#7717=ADVANCED_FACE('',(#1147),#891,.T.);
#7718=ADVANCED_FACE('',(#1148,#765),#892,.T.);
#7719=ADVANCED_FACE('',(#1149),#7386,.T.);
#7720=ADVANCED_FACE('',(#1150,#766),#893,.T.);
#7721=ADVANCED_FACE('',(#1151),#7387,.F.);
#7722=ADVANCED_FACE('',(#1152,#767),#894,.T.);
#7723=ADVANCED_FACE('',(#1153),#7388,.T.);
#7724=ADVANCED_FACE('',(#1154,#768),#895,.T.);
#7725=ADVANCED_FACE('',(#1155),#7389,.F.);
#7726=ADVANCED_FACE('',(#1156),#7390,.F.);
#7727=ADVANCED_FACE('',(#1157),#896,.T.);
#7728=ADVANCED_FACE('',(#1158),#7391,.F.);
#7729=ADVANCED_FACE('',(#1159),#897,.T.);
#7730=ADVANCED_FACE('',(#1160),#7392,.F.);
#7731=ADVANCED_FACE('',(#1161),#898,.T.);
#7732=ADVANCED_FACE('',(#1162),#7393,.F.);
#7733=ADVANCED_FACE('',(#1163),#899,.F.);
#7734=ADVANCED_FACE('',(#1164),#7394,.F.);
#7735=ADVANCED_FACE('',(#1165),#900,.F.);
#7736=ADVANCED_FACE('',(#1166),#7395,.F.);
#7737=ADVANCED_FACE('',(#1167,#769),#901,.T.);
#7738=ADVANCED_FACE('',(#1168),#7396,.F.);
#7739=ADVANCED_FACE('',(#1169),#7397,.F.);
#7740=ADVANCED_FACE('',(#1170,#770),#902,.T.);
#7741=ADVANCED_FACE('',(#1171),#7398,.F.);
#7742=ADVANCED_FACE('',(#1172),#7399,.F.);
#7743=ADVANCED_FACE('',(#1173,#771,#772),#903,.F.);
#7744=ADVANCED_FACE('',(#1174),#904,.F.);
#7745=ADVANCED_FACE('',(#1175),#905,.F.);
#7746=ADVANCED_FACE('',(#1176,#773,#774,#775,#776),#906,.T.);
#7747=ADVANCED_FACE('',(#1177),#907,.F.);
#7748=ADVANCED_FACE('',(#1178,#777,#778),#908,.T.);
#7749=ADVANCED_FACE('',(#1179),#909,.T.);
#7750=ADVANCED_FACE('',(#1180,#779,#780,#781),#910,.T.);
#7751=ADVANCED_FACE('',(#1181),#911,.T.);
#7752=ADVANCED_FACE('',(#1182),#912,.F.);
#7753=ADVANCED_FACE('',(#1183),#913,.T.);
#7754=ADVANCED_FACE('',(#1184),#914,.T.);
#7755=ADVANCED_FACE('',(#1185),#915,.T.);
#7756=ADVANCED_FACE('',(#1186),#916,.T.);
#7757=ADVANCED_FACE('',(#1187),#917,.T.);
#7758=ADVANCED_FACE('',(#1188),#918,.F.);
#7759=ADVANCED_FACE('',(#1189),#919,.T.);
#7760=ADVANCED_FACE('',(#1190,#782,#783),#920,.T.);
#7761=ADVANCED_FACE('',(#1191),#921,.F.);
#7762=ADVANCED_FACE('',(#1192),#922,.F.);
#7763=ADVANCED_FACE('',(#1193,#784,#785),#923,.T.);
#7764=ADVANCED_FACE('',(#1194),#7400,.F.);
#7765=ADVANCED_FACE('',(#1195,#786),#924,.F.);
#7766=ADVANCED_FACE('',(#1196),#7401,.F.);
#7767=ADVANCED_FACE('',(#1197,#787),#925,.F.);
#7768=ADVANCED_FACE('',(#1198),#7402,.F.);
#7769=ADVANCED_FACE('',(#1199),#7403,.F.);
#7770=ADVANCED_FACE('',(#1200),#926,.T.);
#7771=ADVANCED_FACE('',(#1201),#7404,.F.);
#7772=ADVANCED_FACE('',(#1202),#7405,.F.);
#7773=ADVANCED_FACE('',(#1203),#7406,.F.);
#7774=ADVANCED_FACE('',(#1204),#7407,.F.);
#7775=ADVANCED_FACE('',(#1205),#7408,.F.);
#7776=ADVANCED_FACE('',(#1206),#7409,.F.);
#7777=ADVANCED_FACE('',(#1207),#7410,.F.);
#7778=ADVANCED_FACE('',(#1208),#7411,.F.);
#7779=ADVANCED_FACE('',(#1209),#7412,.F.);
#7780=ADVANCED_FACE('',(#1210),#7413,.F.);
#7781=ADVANCED_FACE('',(#1211),#7414,.F.);
#7782=ADVANCED_FACE('',(#1212),#7415,.F.);
#7783=ADVANCED_FACE('',(#1213),#7416,.F.);
#7784=ADVANCED_FACE('',(#1214),#7417,.F.);
#7785=ADVANCED_FACE('',(#1215),#7418,.F.);
#7786=ADVANCED_FACE('',(#1216),#7419,.F.);
#7787=ADVANCED_FACE('',(#1217),#7420,.F.);
#7788=ADVANCED_FACE('',(#1218),#7421,.F.);
#7789=ADVANCED_FACE('',(#1219),#7422,.F.);
#7790=ADVANCED_FACE('',(#1220),#11,.F.);
#7791=ADVANCED_FACE('',(#1221),#12,.F.);
#7792=ADVANCED_FACE('',(#1222,#788,#789,#790,#791),#927,.T.);
#7793=ADVANCED_FACE('',(#1223),#7423,.F.);
#7794=ADVANCED_FACE('',(#1224),#7424,.F.);
#7795=ADVANCED_FACE('',(#1225),#7425,.F.);
#7796=ADVANCED_FACE('',(#1226),#928,.F.);
#7797=ADVANCED_FACE('',(#1227,#792,#793,#794,#795),#929,.F.);
#7798=ADVANCED_FACE('',(#1228),#7426,.T.);
#7799=ADVANCED_FACE('',(#1229),#7427,.F.);
#7800=ADVANCED_FACE('',(#1230),#7428,.T.);
#7801=ADVANCED_FACE('',(#1231,#796),#930,.F.);
#7802=ADVANCED_FACE('',(#1232),#931,.T.);
#7803=ADVANCED_FACE('',(#1233),#566,.T.);
#7804=ADVANCED_FACE('',(#1234),#7429,.T.);
#7805=ADVANCED_FACE('',(#1235),#567,.T.);
#7806=ADVANCED_FACE('',(#1236,#797),#932,.T.);
#7807=ADVANCED_FACE('',(#1237),#568,.T.);
#7808=ADVANCED_FACE('',(#1238),#7430,.T.);
#7809=ADVANCED_FACE('',(#1239),#569,.T.);
#7810=ADVANCED_FACE('',(#1240),#933,.T.);
#7811=ADVANCED_FACE('',(#1241),#934,.F.);
#7812=ADVANCED_FACE('',(#1242),#935,.F.);
#7813=ADVANCED_FACE('',(#1243),#936,.F.);
#7814=ADVANCED_FACE('',(#1244),#937,.F.);
#7815=ADVANCED_FACE('',(#1245),#938,.F.);
#7816=ADVANCED_FACE('',(#1246),#939,.F.);
#7817=ADVANCED_FACE('',(#1247),#940,.F.);
#7818=ADVANCED_FACE('',(#1248),#941,.F.);
#7819=ADVANCED_FACE('',(#1249),#942,.T.);
#7820=ADVANCED_FACE('',(#1250),#570,.T.);
#7821=ADVANCED_FACE('',(#1251),#7431,.T.);
#7822=ADVANCED_FACE('',(#1252),#571,.T.);
#7823=ADVANCED_FACE('',(#1253,#798),#943,.T.);
#7824=ADVANCED_FACE('',(#1254),#572,.T.);
#7825=ADVANCED_FACE('',(#1255),#7432,.T.);
#7826=ADVANCED_FACE('',(#1256),#573,.T.);
#7827=ADVANCED_FACE('',(#1257),#944,.T.);
#7828=ADVANCED_FACE('',(#1258),#945,.F.);
#7829=ADVANCED_FACE('',(#1259),#946,.F.);
#7830=ADVANCED_FACE('',(#1260),#947,.F.);
#7831=ADVANCED_FACE('',(#1261),#948,.F.);
#7832=ADVANCED_FACE('',(#1262),#949,.F.);
#7833=ADVANCED_FACE('',(#1263),#950,.F.);
#7834=ADVANCED_FACE('',(#1264),#951,.F.);
#7835=ADVANCED_FACE('',(#1265),#952,.F.);
#7836=ADVANCED_FACE('',(#1266),#7433,.T.);
#7837=ADVANCED_FACE('',(#1267),#7434,.T.);
#7838=ADVANCED_FACE('',(#1268),#7435,.T.);
#7839=ADVANCED_FACE('',(#1269),#7436,.T.);
#7840=ADVANCED_FACE('',(#1270),#7437,.T.);
#7841=ADVANCED_FACE('',(#1271),#7438,.T.);
#7842=ADVANCED_FACE('',(#1272),#7439,.T.);
#7843=ADVANCED_FACE('',(#1273),#7440,.T.);
#7844=ADVANCED_FACE('',(#1274),#7441,.T.);
#7845=ADVANCED_FACE('',(#1275),#7442,.T.);
#7846=ADVANCED_FACE('',(#1276),#7443,.T.);
#7847=ADVANCED_FACE('',(#1277),#7444,.T.);
#7848=ADVANCED_FACE('',(#1278),#7445,.T.);
#7849=ADVANCED_FACE('',(#1279),#7446,.T.);
#7850=ADVANCED_FACE('',(#1280),#7447,.T.);
#7851=ADVANCED_FACE('',(#1281),#7448,.T.);
#7852=ADVANCED_FACE('',(#1282),#7449,.T.);
#7853=ADVANCED_FACE('',(#1283),#7450,.T.);
#7854=ADVANCED_FACE('',(#1284),#7451,.T.);
#7855=ADVANCED_FACE('',(#1285),#7452,.T.);
#7856=ADVANCED_FACE('',(#1286),#7453,.T.);
#7857=ADVANCED_FACE('',(#1287),#7454,.T.);
#7858=ADVANCED_FACE('',(#1288),#7455,.T.);
#7859=ADVANCED_FACE('',(#1289),#7456,.T.);
#7860=ADVANCED_FACE('',(#1290),#7457,.T.);
#7861=ADVANCED_FACE('',(#1291),#7458,.T.);
#7862=ADVANCED_FACE('',(#1292),#7459,.T.);
#7863=ADVANCED_FACE('',(#1293),#7460,.T.);
#7864=ADVANCED_FACE('',(#1294),#7461,.T.);
#7865=ADVANCED_FACE('',(#1295),#7462,.T.);
#7866=ADVANCED_FACE('',(#1296),#7463,.T.);
#7867=ADVANCED_FACE('',(#1297),#7464,.T.);
#7868=ADVANCED_FACE('',(#1298),#7465,.T.);
#7869=ADVANCED_FACE('',(#1299),#7466,.T.);
#7870=ADVANCED_FACE('',(#1300),#7467,.T.);
#7871=ADVANCED_FACE('',(#1301),#7468,.T.);
#7872=ADVANCED_FACE('',(#1302),#7469,.T.);
#7873=ADVANCED_FACE('',(#1303),#7470,.T.);
#7874=ADVANCED_FACE('',(#1304),#7471,.T.);
#7875=ADVANCED_FACE('',(#1305),#7472,.T.);
#7876=ADVANCED_FACE('',(#1306),#7473,.T.);
#7877=ADVANCED_FACE('',(#1307),#7474,.T.);
#7878=ADVANCED_FACE('',(#1308),#7475,.T.);
#7879=ADVANCED_FACE('',(#1309),#7476,.T.);
#7880=ADVANCED_FACE('',(#1310),#7477,.T.);
#7881=ADVANCED_FACE('',(#1311),#7478,.T.);
#7882=ADVANCED_FACE('',(#1312),#7479,.T.);
#7883=ADVANCED_FACE('',(#1313),#7480,.T.);
#7884=ADVANCED_FACE('',(#1314),#7481,.T.);
#7885=ADVANCED_FACE('',(#1315),#7482,.T.);
#7886=ADVANCED_FACE('',(#1316),#7483,.T.);
#7887=ADVANCED_FACE('',(#1317),#7484,.T.);
#7888=ADVANCED_FACE('',(#1318),#7485,.T.);
#7889=ADVANCED_FACE('',(#1319),#7486,.T.);
#7890=ADVANCED_FACE('',(#1320),#7487,.T.);
#7891=ADVANCED_FACE('',(#1321),#7488,.T.);
#7892=ADVANCED_FACE('',(#1322),#7489,.T.);
#7893=ADVANCED_FACE('',(#1323),#7490,.T.);
#7894=ADVANCED_FACE('',(#1324),#7491,.T.);
#7895=ADVANCED_FACE('',(#1325),#7492,.T.);
#7896=ADVANCED_FACE('',(#1326),#7493,.T.);
#7897=ADVANCED_FACE('',(#1327),#7494,.T.);
#7898=ADVANCED_FACE('',(#1328),#7495,.T.);
#7899=ADVANCED_FACE('',(#1329),#7496,.T.);
#7900=ADVANCED_FACE('',(#1330),#7497,.T.);
#7901=ADVANCED_FACE('',(#1331),#7498,.T.);
#7902=ADVANCED_FACE('',(#1332),#7499,.T.);
#7903=ADVANCED_FACE('',(#1333),#7500,.T.);
#7904=ADVANCED_FACE('',(#1334),#7501,.T.);
#7905=ADVANCED_FACE('',(#1335),#7502,.T.);
#7906=ADVANCED_FACE('',(#1336),#7503,.T.);
#7907=ADVANCED_FACE('',(#1337),#7504,.T.);
#7908=ADVANCED_FACE('',(#1338),#7505,.T.);
#7909=ADVANCED_FACE('',(#1339),#7506,.T.);
#7910=ADVANCED_FACE('',(#1340),#7507,.T.);
#7911=ADVANCED_FACE('',(#1341),#7508,.T.);
#7912=ADVANCED_FACE('',(#1342),#7509,.T.);
#7913=ADVANCED_FACE('',(#1343),#7510,.T.);
#7914=ADVANCED_FACE('',(#1344),#7511,.T.);
#7915=ADVANCED_FACE('',(#1345),#7512,.T.);
#7916=ADVANCED_FACE('',(#1346),#7513,.T.);
#7917=ADVANCED_FACE('',(#1347),#7514,.T.);
#7918=ADVANCED_FACE('',(#1348),#7515,.T.);
#7919=ADVANCED_FACE('',(#1349),#7516,.T.);
#7920=ADVANCED_FACE('',(#1350),#7517,.T.);
#7921=ADVANCED_FACE('',(#1351),#7518,.T.);
#7922=ADVANCED_FACE('',(#1352),#7519,.T.);
#7923=ADVANCED_FACE('',(#1353),#7520,.T.);
#7924=ADVANCED_FACE('',(#1354),#7521,.T.);
#7925=ADVANCED_FACE('',(#1355),#7522,.T.);
#7926=ADVANCED_FACE('',(#1356),#7523,.T.);
#7927=ADVANCED_FACE('',(#1357),#7524,.T.);
#7928=ADVANCED_FACE('',(#1358),#7525,.T.);
#7929=ADVANCED_FACE('',(#1359),#7526,.T.);
#7930=ADVANCED_FACE('',(#1360),#7527,.T.);
#7931=ADVANCED_FACE('',(#1361),#7528,.T.);
#7932=ADVANCED_FACE('',(#1362),#7529,.T.);
#7933=ADVANCED_FACE('',(#1363),#7530,.T.);
#7934=ADVANCED_FACE('',(#1364),#7531,.T.);
#7935=ADVANCED_FACE('',(#1365),#7532,.T.);
#7936=ADVANCED_FACE('',(#1366),#7533,.T.);
#7937=ADVANCED_FACE('',(#1367),#7534,.T.);
#7938=ADVANCED_FACE('',(#1368),#7535,.T.);
#7939=ADVANCED_FACE('',(#1369),#7536,.T.);
#7940=ADVANCED_FACE('',(#1370),#7537,.T.);
#7941=ADVANCED_FACE('',(#1371),#7538,.T.);
#7942=ADVANCED_FACE('',(#1372),#7539,.T.);
#7943=ADVANCED_FACE('',(#1373),#7540,.T.);
#7944=ADVANCED_FACE('',(#1374),#7541,.T.);
#7945=ADVANCED_FACE('',(#1375),#7542,.T.);
#7946=ADVANCED_FACE('',(#1376),#7543,.T.);
#7947=ADVANCED_FACE('',(#1377),#7544,.T.);
#7948=ADVANCED_FACE('',(#1378),#7545,.T.);
#7949=ADVANCED_FACE('',(#1379),#7546,.T.);
#7950=ADVANCED_FACE('',(#1380),#7547,.T.);
#7951=ADVANCED_FACE('',(#1381),#7548,.T.);
#7952=ADVANCED_FACE('',(#1382),#7549,.T.);
#7953=ADVANCED_FACE('',(#1383),#7550,.T.);
#7954=ADVANCED_FACE('',(#1384),#7551,.T.);
#7955=ADVANCED_FACE('',(#1385),#7552,.T.);
#7956=ADVANCED_FACE('',(#1386),#7553,.T.);
#7957=ADVANCED_FACE('',(#1387),#7554,.T.);
#7958=ADVANCED_FACE('',(#1388),#7555,.T.);
#7959=ADVANCED_FACE('',(#1389),#7556,.T.);
#7960=ADVANCED_FACE('',(#1390),#7557,.T.);
#7961=ADVANCED_FACE('',(#1391),#7558,.T.);
#7962=ADVANCED_FACE('',(#1392),#13,.F.);
#7963=ADVANCED_FACE('',(#1393),#7559,.T.);
#7964=ADVANCED_FACE('',(#1394),#14,.F.);
#7965=ADVANCED_FACE('',(#1395),#953,.F.);
#7966=ADVANCED_FACE('',(#1396),#954,.T.);
#7967=ADVANCED_FACE('',(#1397),#955,.F.);
#7968=ADVANCED_FACE('',(#1398),#956,.F.);
#7969=ADVANCED_FACE('',(#1399),#957,.F.);
#7970=ADVANCED_FACE('',(#1400,#799),#7560,.T.);
#7971=ADVANCED_FACE('',(#1401),#958,.T.);
#7972=ADVANCED_FACE('',(#1402,#800),#959,.F.);
#7973=ADVANCED_FACE('',(#1403),#7561,.T.);
#7974=ADVANCED_FACE('',(#1404,#801),#960,.T.);
#7975=ADVANCED_FACE('',(#1405),#7562,.T.);
#7976=ADVANCED_FACE('',(#1406),#961,.F.);
#7977=ADVANCED_FACE('',(#1407),#7563,.F.);
#7978=ADVANCED_FACE('',(#1408),#7564,.T.);
#7979=ADVANCED_FACE('',(#1409,#802),#962,.T.);
#7980=ADVANCED_FACE('',(#1410,#803),#963,.F.);
#7981=ADVANCED_FACE('',(#1411),#964,.T.);
#7982=ADVANCED_FACE('',(#1412),#7565,.F.);
#7983=ADVANCED_FACE('',(#1413),#965,.T.);
#7984=ADVANCED_FACE('',(#1414,#804),#7566,.F.);
#7985=ADVANCED_FACE('',(#1415,#805),#7567,.T.);
#7986=ADVANCED_FACE('',(#1416,#806),#966,.T.);
#7987=ADVANCED_FACE('',(#1417,#807),#967,.F.);
#7988=ADVANCED_FACE('',(#1418),#7568,.F.);
#7989=ADVANCED_FACE('',(#1419),#968,.T.);
#7990=ADVANCED_FACE('',(#1420),#7569,.F.);
#7991=ADVANCED_FACE('',(#1421),#969,.T.);
#7992=ADVANCED_FACE('',(#1422),#970,.F.);
#7993=ADVANCED_FACE('',(#1423),#971,.F.);
#7994=ADVANCED_FACE('',(#1424),#972,.F.);
#7995=ADVANCED_FACE('',(#1425,#808,#809),#973,.T.);
#7996=ADVANCED_FACE('',(#1426,#810,#811),#974,.F.);
#7997=ADVANCED_FACE('',(#1427),#7570,.T.);
#7998=ADVANCED_FACE('',(#1428,#812),#7571,.F.);
#7999=ADVANCED_FACE('',(#1429,#813),#7572,.T.);
#8000=ADVANCED_FACE('',(#1430),#975,.F.);
#8001=ADVANCED_FACE('',(#1431),#7573,.F.);
#8002=ADVANCED_FACE('',(#1432),#7574,.T.);
#8003=ADVANCED_FACE('',(#1433,#814),#976,.T.);
#8004=ADVANCED_FACE('',(#1434,#815),#977,.F.);
#8005=ADVANCED_FACE('',(#1435),#7575,.F.);
#8006=ADVANCED_FACE('',(#1436),#7576,.T.);
#8007=ADVANCED_FACE('',(#1437,#816),#978,.T.);
#8008=ADVANCED_FACE('',(#1438,#817),#979,.F.);
#8009=ADVANCED_FACE('',(#1439),#980,.F.);
#8010=ADVANCED_FACE('',(#1440),#981,.T.);
#8011=ADVANCED_FACE('',(#1441),#982,.T.);
#8012=ADVANCED_FACE('',(#1442),#983,.T.);
#8013=ADVANCED_FACE('',(#1443),#984,.T.);
#8014=ADVANCED_FACE('',(#1444),#985,.T.);
#8015=ADVANCED_FACE('',(#1445),#986,.F.);
#8016=ADVANCED_FACE('',(#1446),#987,.T.);
#8017=ADVANCED_FACE('',(#1447),#988,.T.);
#8018=ADVANCED_FACE('',(#1448),#989,.T.);
#8019=ADVANCED_FACE('',(#1449),#990,.F.);
#8020=ADVANCED_FACE('',(#1450),#991,.F.);
#8021=ADVANCED_FACE('',(#1451),#992,.F.);
#8022=ADVANCED_FACE('',(#1452),#993,.F.);
#8023=ADVANCED_FACE('',(#1453),#994,.F.);
#8024=ADVANCED_FACE('',(#1454),#995,.F.);
#8025=ADVANCED_FACE('',(#1455),#996,.F.);
#8026=ADVANCED_FACE('',(#1456,#818),#997,.T.);
#8027=ADVANCED_FACE('',(#1457),#574,.T.);
#8028=ADVANCED_FACE('',(#1458),#7577,.T.);
#8029=ADVANCED_FACE('',(#1459),#575,.T.);
#8030=ADVANCED_FACE('',(#1460),#998,.T.);
#8031=ADVANCED_FACE('',(#1461),#7578,.F.);
#8032=ADVANCED_FACE('',(#1462),#7579,.T.);
#8033=ADVANCED_FACE('',(#1463,#819),#999,.T.);
#8034=ADVANCED_FACE('',(#1464,#820),#1000,.F.);
#8035=ADVANCED_FACE('',(#1465),#1001,.T.);
#8036=ADVANCED_FACE('',(#1466),#576,.T.);
#8037=ADVANCED_FACE('',(#1467),#7580,.T.);
#8038=ADVANCED_FACE('',(#1468),#577,.T.);
#8039=ADVANCED_FACE('',(#1469,#821),#1002,.T.);
#8040=ADVANCED_FACE('',(#1470),#578,.T.);
#8041=ADVANCED_FACE('',(#1471),#7581,.T.);
#8042=ADVANCED_FACE('',(#1472),#579,.T.);
#8043=ADVANCED_FACE('',(#1473),#1003,.T.);
#8044=ADVANCED_FACE('',(#1474),#1004,.F.);
#8045=ADVANCED_FACE('',(#1475),#1005,.F.);
#8046=ADVANCED_FACE('',(#1476),#1006,.F.);
#8047=ADVANCED_FACE('',(#1477),#1007,.F.);
#8048=ADVANCED_FACE('',(#1478),#1008,.F.);
#8049=ADVANCED_FACE('',(#1479),#1009,.F.);
#8050=ADVANCED_FACE('',(#1480),#1010,.F.);
#8051=ADVANCED_FACE('',(#1481),#1011,.F.);
#8052=CLOSED_SHELL('',(#7582,#7583,#7584,#7585,#7586,#7587,#7588,#7589,
#7590,#7591,#7592,#7593,#7594));
#8053=CLOSED_SHELL('',(#7595,#7596,#7597,#7598,#7599,#7600,#7601,#7602,
#7603,#7604,#7605,#7606));
#8054=CLOSED_SHELL('',(#7607,#7608,#7609,#7610,#7611,#7612,#7613,#7614,
#7615,#7616,#7617,#7618,#7619,#7620));
#8055=CLOSED_SHELL('',(#7621,#7622,#7623,#7624,#7625,#7626,#7627,#7628,
#7629,#7630,#7631,#7632,#7633,#7634,#7635,#7636));
#8056=CLOSED_SHELL('',(#7637,#7638,#7639,#7640,#7641,#7642,#7643,#7644,
#7645,#7646));
#8057=CLOSED_SHELL('',(#7647,#7648,#7649,#7650,#7651,#7652,#7653,#7654,
#7655,#7656,#7657,#7658));
#8058=CLOSED_SHELL('',(#7659,#7660,#7661,#7662,#7663,#7664,#7665,#7666));
#8059=CLOSED_SHELL('',(#7667,#7668,#7669,#7670,#7671,#7672,#7673,#7674));
#8060=CLOSED_SHELL('',(#7675,#7676,#7677,#7678,#7679,#7680,#7681,#7682));
#8061=CLOSED_SHELL('',(#7683,#7684,#7685,#7686,#7687,#7688,#7689,#7690));
#8062=CLOSED_SHELL('',(#7691));
#8063=CLOSED_SHELL('',(#7692));
#8064=CLOSED_SHELL('',(#7693));
#8065=CLOSED_SHELL('',(#7694));
#8066=CLOSED_SHELL('',(#7695));
#8067=CLOSED_SHELL('',(#7696));
#8068=CLOSED_SHELL('',(#7697));
#8069=CLOSED_SHELL('',(#7698));
#8070=CLOSED_SHELL('',(#7699,#7700,#7701,#7702,#7703,#7704,#7705,#7706,
#7707,#7708,#7709,#7710,#7711,#7712,#7713,#7714,#7715,#7716,#7717));
#8071=CLOSED_SHELL('',(#7718,#7719,#7720,#7721));
#8072=CLOSED_SHELL('',(#7722,#7723,#7724,#7725));
#8073=CLOSED_SHELL('',(#7726,#7727,#7728,#7729,#7730,#7731,#7732,#7733,
#7734,#7735,#7736,#7737,#7738,#7739,#7740,#7741,#7742,#7743,#7744,#7745,
#7746,#7747,#7748,#7749,#7750,#7751,#7752));
#8074=CLOSED_SHELL('',(#7753,#7754,#7755,#7756,#7757,#7758));
#8075=CLOSED_SHELL('',(#7759,#7760,#7761,#7762,#7763,#7764,#7765,#7766,
#7767,#7768,#7769,#7770));
#8076=CLOSED_SHELL('',(#7771,#7772,#7773,#7774,#7775,#7776,#7777,#7778,
#7779,#7780,#7781,#7782,#7783,#7784,#7785,#7786,#7787,#7788,#7789,#7790,
#7791,#7792,#7793,#7794,#7795,#7796,#7797,#7798,#7799,#7800,#7801));
#8077=CLOSED_SHELL('',(#7802,#7803,#7804,#7805,#7806,#7807,#7808,#7809,
#7810));
#8078=CLOSED_SHELL('',(#7811,#7812,#7813,#7814,#7815,#7816,#7817,#7818));
#8079=CLOSED_SHELL('',(#7819,#7820,#7821,#7822,#7823,#7824,#7825,#7826,
#7827));
#8080=CLOSED_SHELL('',(#7828,#7829,#7830,#7831,#7832,#7833,#7834,#7835));
#8081=CLOSED_SHELL('',(#7836,#7837,#7838,#7839,#7840,#7841,#7842,#7843,
#7844,#7845,#7846,#7847,#7848,#7849,#7850,#7851,#7852,#7853,#7854,#7855,
#7856,#7857,#7858,#7859,#7860,#7861,#7862,#7863,#7864,#7865,#7866,#7867,
#7868,#7869,#7870,#7871,#7872,#7873,#7874,#7875,#7876,#7877,#7878,#7879,
#7880,#7881,#7882,#7883,#7884,#7885,#7886,#7887,#7888,#7889,#7890,#7891,
#7892,#7893,#7894,#7895,#7896,#7897,#7898,#7899,#7900,#7901,#7902,#7903,
#7904,#7905,#7906,#7907,#7908,#7909,#7910,#7911,#7912,#7913,#7914,#7915,
#7916,#7917,#7918,#7919,#7920,#7921,#7922,#7923,#7924,#7925,#7926,#7927,
#7928,#7929,#7930,#7931,#7932,#7933,#7934,#7935,#7936,#7937,#7938,#7939,
#7940,#7941,#7942,#7943,#7944,#7945,#7946,#7947,#7948,#7949,#7950,#7951,
#7952,#7953,#7954,#7955,#7956,#7957,#7958,#7959,#7960,#7961,#7962,#7963,
#7964,#7965,#7966,#7967,#7968,#7969,#7970,#7971,#7972,#7973,#7974,#7975,
#7976));
#8082=CLOSED_SHELL('',(#7977,#7978,#7979,#7980));
#8083=CLOSED_SHELL('',(#7981,#7982,#7983,#7984,#7985,#7986,#7987));
#8084=CLOSED_SHELL('',(#7988,#7989,#7990,#7991,#7992,#7993,#7994,#7995,
#7996,#7997,#7998,#7999,#8000));
#8085=CLOSED_SHELL('',(#8001,#8002,#8003,#8004));
#8086=CLOSED_SHELL('',(#8005,#8006,#8007,#8008));
#8087=CLOSED_SHELL('',(#8009,#8010,#8011,#8012,#8013,#8014,#8015,#8016,
#8017,#8018));
#8088=CLOSED_SHELL('',(#8019,#8020,#8021,#8022,#8023,#8024,#8025,#8026,
#8027,#8028,#8029,#8030));
#8089=CLOSED_SHELL('',(#8031,#8032,#8033,#8034));
#8090=CLOSED_SHELL('',(#8035,#8036,#8037,#8038,#8039,#8040,#8041,#8042,
#8043));
#8091=CLOSED_SHELL('',(#8044,#8045,#8046,#8047,#8048,#8049,#8050,#8051));
#8092=DERIVED_UNIT_ELEMENT(#8148,1.);
#8093=DERIVED_UNIT_ELEMENT(#25076,-3.);
#8094=DERIVED_UNIT_ELEMENT(#8148,1.);
#8095=DERIVED_UNIT_ELEMENT(#25076,-3.);
#8096=DERIVED_UNIT_ELEMENT(#8148,1.);
#8097=DERIVED_UNIT_ELEMENT(#25076,-3.);
#8098=DERIVED_UNIT_ELEMENT(#8148,1.);
#8099=DERIVED_UNIT_ELEMENT(#25076,-3.);
#8100=DERIVED_UNIT_ELEMENT(#8148,1.);
#8101=DERIVED_UNIT_ELEMENT(#25076,-3.);
#8102=DERIVED_UNIT_ELEMENT(#8148,1.);
#8103=DERIVED_UNIT_ELEMENT(#25076,-3.);
#8104=DERIVED_UNIT_ELEMENT(#8148,1.);
#8105=DERIVED_UNIT_ELEMENT(#25076,-3.);
#8106=DERIVED_UNIT_ELEMENT(#8148,1.);
#8107=DERIVED_UNIT_ELEMENT(#25076,-3.);
#8108=DERIVED_UNIT_ELEMENT(#8148,1.);
#8109=DERIVED_UNIT_ELEMENT(#25076,-3.);
#8110=DERIVED_UNIT_ELEMENT(#8148,1.);
#8111=DERIVED_UNIT_ELEMENT(#25076,-3.);
#8112=DERIVED_UNIT_ELEMENT(#8148,1.);
#8113=DERIVED_UNIT_ELEMENT(#25076,-3.);
#8114=DERIVED_UNIT_ELEMENT(#8148,1.);
#8115=DERIVED_UNIT_ELEMENT(#25076,-3.);
#8116=DERIVED_UNIT_ELEMENT(#8148,1.);
#8117=DERIVED_UNIT_ELEMENT(#25076,-3.);
#8118=DERIVED_UNIT_ELEMENT(#8148,1.);
#8119=DERIVED_UNIT_ELEMENT(#25076,-3.);
#8120=DERIVED_UNIT_ELEMENT(#8148,1.);
#8121=DERIVED_UNIT_ELEMENT(#25076,-3.);
#8122=DERIVED_UNIT_ELEMENT(#8148,1.);
#8123=DERIVED_UNIT_ELEMENT(#25076,-3.);
#8124=DERIVED_UNIT_ELEMENT(#8148,1.);
#8125=DERIVED_UNIT_ELEMENT(#25076,-3.);
#8126=DERIVED_UNIT_ELEMENT(#8148,1.);
#8127=DERIVED_UNIT_ELEMENT(#25076,-3.);
#8128=DERIVED_UNIT_ELEMENT(#8148,1.);
#8129=DERIVED_UNIT_ELEMENT(#25076,-3.);
#8130=DERIVED_UNIT_ELEMENT(#8148,1.);
#8131=DERIVED_UNIT_ELEMENT(#25076,-3.);
#8132=DERIVED_UNIT_ELEMENT(#8148,1.);
#8133=DERIVED_UNIT_ELEMENT(#25076,-3.);
#8134=DERIVED_UNIT_ELEMENT(#8148,1.);
#8135=DERIVED_UNIT_ELEMENT(#25076,-3.);
#8136=DERIVED_UNIT_ELEMENT(#8148,1.);
#8137=DERIVED_UNIT_ELEMENT(#25076,-3.);
#8138=DERIVED_UNIT_ELEMENT(#8148,1.);
#8139=DERIVED_UNIT_ELEMENT(#25076,-3.);
#8140=DERIVED_UNIT_ELEMENT(#8148,1.);
#8141=DERIVED_UNIT_ELEMENT(#25076,-3.);
#8142=DERIVED_UNIT_ELEMENT(#8148,1.);
#8143=DERIVED_UNIT_ELEMENT(#25076,-3.);
#8144=DERIVED_UNIT_ELEMENT(#8148,1.);
#8145=DERIVED_UNIT_ELEMENT(#25076,-3.);
#8146=DERIVED_UNIT_ELEMENT(#8148,1.);
#8147=DERIVED_UNIT_ELEMENT(#25076,-3.);
#8148=(
MASS_UNIT()
NAMED_UNIT(*)
SI_UNIT(.KILO.,.GRAM.)
);
#8149=DERIVED_UNIT((#8092,#8093));
#8150=DERIVED_UNIT((#8094,#8095));
#8151=DERIVED_UNIT((#8096,#8097));
#8152=DERIVED_UNIT((#8098,#8099));
#8153=DERIVED_UNIT((#8100,#8101));
#8154=DERIVED_UNIT((#8102,#8103));
#8155=DERIVED_UNIT((#8104,#8105));
#8156=DERIVED_UNIT((#8106,#8107));
#8157=DERIVED_UNIT((#8108,#8109));
#8158=DERIVED_UNIT((#8110,#8111));
#8159=DERIVED_UNIT((#8112,#8113));
#8160=DERIVED_UNIT((#8114,#8115));
#8161=DERIVED_UNIT((#8116,#8117));
#8162=DERIVED_UNIT((#8118,#8119));
#8163=DERIVED_UNIT((#8120,#8121));
#8164=DERIVED_UNIT((#8122,#8123));
#8165=DERIVED_UNIT((#8124,#8125));
#8166=DERIVED_UNIT((#8126,#8127));
#8167=DERIVED_UNIT((#8128,#8129));
#8168=DERIVED_UNIT((#8130,#8131));
#8169=DERIVED_UNIT((#8132,#8133));
#8170=DERIVED_UNIT((#8134,#8135));
#8171=DERIVED_UNIT((#8136,#8137));
#8172=DERIVED_UNIT((#8138,#8139));
#8173=DERIVED_UNIT((#8140,#8141));
#8174=DERIVED_UNIT((#8142,#8143));
#8175=DERIVED_UNIT((#8144,#8145));
#8176=DERIVED_UNIT((#8146,#8147));
#8177=MEASURE_REPRESENTATION_ITEM('density measure',
POSITIVE_RATIO_MEASURE(7850.),#8149);
#8178=MEASURE_REPRESENTATION_ITEM('density measure',
POSITIVE_RATIO_MEASURE(7850.),#8150);
#8179=MEASURE_REPRESENTATION_ITEM('density measure',
POSITIVE_RATIO_MEASURE(7850.),#8151);
#8180=MEASURE_REPRESENTATION_ITEM('density measure',
POSITIVE_RATIO_MEASURE(7850.),#8152);
#8181=MEASURE_REPRESENTATION_ITEM('density measure',
POSITIVE_RATIO_MEASURE(7850.),#8153);
#8182=MEASURE_REPRESENTATION_ITEM('density measure',
POSITIVE_RATIO_MEASURE(7850.),#8154);
#8183=MEASURE_REPRESENTATION_ITEM('density measure',
POSITIVE_RATIO_MEASURE(7850.),#8155);
#8184=MEASURE_REPRESENTATION_ITEM('density measure',
POSITIVE_RATIO_MEASURE(7850.),#8156);
#8185=MEASURE_REPRESENTATION_ITEM('density measure',
POSITIVE_RATIO_MEASURE(7850.),#8157);
#8186=MEASURE_REPRESENTATION_ITEM('density measure',
POSITIVE_RATIO_MEASURE(7850.),#8158);
#8187=MEASURE_REPRESENTATION_ITEM('density measure',
POSITIVE_RATIO_MEASURE(7850.),#8159);
#8188=MEASURE_REPRESENTATION_ITEM('density measure',
POSITIVE_RATIO_MEASURE(7850.),#8160);
#8189=MEASURE_REPRESENTATION_ITEM('density measure',
POSITIVE_RATIO_MEASURE(7850.),#8161);
#8190=MEASURE_REPRESENTATION_ITEM('density measure',
POSITIVE_RATIO_MEASURE(7850.),#8162);
#8191=MEASURE_REPRESENTATION_ITEM('density measure',
POSITIVE_RATIO_MEASURE(7850.),#8163);
#8192=MEASURE_REPRESENTATION_ITEM('density measure',
POSITIVE_RATIO_MEASURE(7850.),#8164);
#8193=MEASURE_REPRESENTATION_ITEM('density measure',
POSITIVE_RATIO_MEASURE(7850.),#8165);
#8194=MEASURE_REPRESENTATION_ITEM('density measure',
POSITIVE_RATIO_MEASURE(7850.),#8166);
#8195=MEASURE_REPRESENTATION_ITEM('density measure',
POSITIVE_RATIO_MEASURE(7850.),#8167);
#8196=MEASURE_REPRESENTATION_ITEM('density measure',
POSITIVE_RATIO_MEASURE(7850.),#8168);
#8197=MEASURE_REPRESENTATION_ITEM('density measure',
POSITIVE_RATIO_MEASURE(7850.),#8169);
#8198=MEASURE_REPRESENTATION_ITEM('density measure',
POSITIVE_RATIO_MEASURE(7850.),#8170);
#8199=MEASURE_REPRESENTATION_ITEM('density measure',
POSITIVE_RATIO_MEASURE(7850.),#8171);
#8200=MEASURE_REPRESENTATION_ITEM('density measure',
POSITIVE_RATIO_MEASURE(7850.),#8172);
#8201=MEASURE_REPRESENTATION_ITEM('density measure',
POSITIVE_RATIO_MEASURE(7850.),#8173);
#8202=MEASURE_REPRESENTATION_ITEM('density measure',
POSITIVE_RATIO_MEASURE(7850.),#8174);
#8203=MEASURE_REPRESENTATION_ITEM('density measure',
POSITIVE_RATIO_MEASURE(7850.),#8175);
#8204=MEASURE_REPRESENTATION_ITEM('density measure',
POSITIVE_RATIO_MEASURE(7850.),#8176);
#8205=PROPERTY_DEFINITION_REPRESENTATION(#8345,#8261);
#8206=PROPERTY_DEFINITION_REPRESENTATION(#8346,#8262);
#8207=PROPERTY_DEFINITION_REPRESENTATION(#8347,#8263);
#8208=PROPERTY_DEFINITION_REPRESENTATION(#8348,#8264);
#8209=PROPERTY_DEFINITION_REPRESENTATION(#8349,#8265);
#8210=PROPERTY_DEFINITION_REPRESENTATION(#8350,#8266);
#8211=PROPERTY_DEFINITION_REPRESENTATION(#8351,#8267);
#8212=PROPERTY_DEFINITION_REPRESENTATION(#8352,#8268);
#8213=PROPERTY_DEFINITION_REPRESENTATION(#8353,#8269);
#8214=PROPERTY_DEFINITION_REPRESENTATION(#8354,#8270);
#8215=PROPERTY_DEFINITION_REPRESENTATION(#8355,#8271);
#8216=PROPERTY_DEFINITION_REPRESENTATION(#8356,#8272);
#8217=PROPERTY_DEFINITION_REPRESENTATION(#8357,#8273);
#8218=PROPERTY_DEFINITION_REPRESENTATION(#8358,#8274);
#8219=PROPERTY_DEFINITION_REPRESENTATION(#8359,#8275);
#8220=PROPERTY_DEFINITION_REPRESENTATION(#8360,#8276);
#8221=PROPERTY_DEFINITION_REPRESENTATION(#8361,#8277);
#8222=PROPERTY_DEFINITION_REPRESENTATION(#8362,#8278);
#8223=PROPERTY_DEFINITION_REPRESENTATION(#8363,#8279);
#8224=PROPERTY_DEFINITION_REPRESENTATION(#8364,#8280);
#8225=PROPERTY_DEFINITION_REPRESENTATION(#8365,#8281);
#8226=PROPERTY_DEFINITION_REPRESENTATION(#8366,#8282);
#8227=PROPERTY_DEFINITION_REPRESENTATION(#8367,#8283);
#8228=PROPERTY_DEFINITION_REPRESENTATION(#8368,#8284);
#8229=PROPERTY_DEFINITION_REPRESENTATION(#8369,#8285);
#8230=PROPERTY_DEFINITION_REPRESENTATION(#8370,#8286);
#8231=PROPERTY_DEFINITION_REPRESENTATION(#8371,#8287);
#8232=PROPERTY_DEFINITION_REPRESENTATION(#8372,#8288);
#8233=PROPERTY_DEFINITION_REPRESENTATION(#8373,#8289);
#8234=PROPERTY_DEFINITION_REPRESENTATION(#8374,#8290);
#8235=PROPERTY_DEFINITION_REPRESENTATION(#8375,#8291);
#8236=PROPERTY_DEFINITION_REPRESENTATION(#8376,#8292);
#8237=PROPERTY_DEFINITION_REPRESENTATION(#8377,#8293);
#8238=PROPERTY_DEFINITION_REPRESENTATION(#8378,#8294);
#8239=PROPERTY_DEFINITION_REPRESENTATION(#8379,#8295);
#8240=PROPERTY_DEFINITION_REPRESENTATION(#8380,#8296);
#8241=PROPERTY_DEFINITION_REPRESENTATION(#8381,#8297);
#8242=PROPERTY_DEFINITION_REPRESENTATION(#8382,#8298);
#8243=PROPERTY_DEFINITION_REPRESENTATION(#8383,#8299);
#8244=PROPERTY_DEFINITION_REPRESENTATION(#8384,#8300);
#8245=PROPERTY_DEFINITION_REPRESENTATION(#8385,#8301);
#8246=PROPERTY_DEFINITION_REPRESENTATION(#8386,#8302);
#8247=PROPERTY_DEFINITION_REPRESENTATION(#8387,#8303);
#8248=PROPERTY_DEFINITION_REPRESENTATION(#8388,#8304);
#8249=PROPERTY_DEFINITION_REPRESENTATION(#8389,#8305);
#8250=PROPERTY_DEFINITION_REPRESENTATION(#8390,#8306);
#8251=PROPERTY_DEFINITION_REPRESENTATION(#8391,#8307);
#8252=PROPERTY_DEFINITION_REPRESENTATION(#8392,#8308);
#8253=PROPERTY_DEFINITION_REPRESENTATION(#8393,#8309);
#8254=PROPERTY_DEFINITION_REPRESENTATION(#8394,#8310);
#8255=PROPERTY_DEFINITION_REPRESENTATION(#8395,#8311);
#8256=PROPERTY_DEFINITION_REPRESENTATION(#8396,#8312);
#8257=PROPERTY_DEFINITION_REPRESENTATION(#8397,#8313);
#8258=PROPERTY_DEFINITION_REPRESENTATION(#8398,#8314);
#8259=PROPERTY_DEFINITION_REPRESENTATION(#8399,#8315);
#8260=PROPERTY_DEFINITION_REPRESENTATION(#8400,#8316);
#8261=REPRESENTATION('material name',(#8317),#25043);
#8262=REPRESENTATION('density',(#8177),#25043);
#8263=REPRESENTATION('material name',(#8318),#25044);
#8264=REPRESENTATION('density',(#8178),#25044);
#8265=REPRESENTATION('material name',(#8319),#25045);
#8266=REPRESENTATION('density',(#8179),#25045);
#8267=REPRESENTATION('material name',(#8320),#25046);
#8268=REPRESENTATION('density',(#8180),#25046);
#8269=REPRESENTATION('material name',(#8321),#25047);
#8270=REPRESENTATION('density',(#8181),#25047);
#8271=REPRESENTATION('material name',(#8322),#25048);
#8272=REPRESENTATION('density',(#8182),#25048);
#8273=REPRESENTATION('material name',(#8323),#25049);
#8274=REPRESENTATION('density',(#8183),#25049);
#8275=REPRESENTATION('material name',(#8324),#25051);
#8276=REPRESENTATION('density',(#8184),#25051);
#8277=REPRESENTATION('material name',(#8325),#25052);
#8278=REPRESENTATION('density',(#8185),#25052);
#8279=REPRESENTATION('material name',(#8326),#25053);
#8280=REPRESENTATION('density',(#8186),#25053);
#8281=REPRESENTATION('material name',(#8327),#25054);
#8282=REPRESENTATION('density',(#8187),#25054);
#8283=REPRESENTATION('material name',(#8328),#25055);
#8284=REPRESENTATION('density',(#8188),#25055);
#8285=REPRESENTATION('material name',(#8329),#25057);
#8286=REPRESENTATION('density',(#8189),#25057);
#8287=REPRESENTATION('material name',(#8330),#25058);
#8288=REPRESENTATION('density',(#8190),#25058);
#8289=REPRESENTATION('material name',(#8331),#25059);
#8290=REPRESENTATION('density',(#8191),#25059);
#8291=REPRESENTATION('material name',(#8332),#25060);
#8292=REPRESENTATION('density',(#8192),#25060);
#8293=REPRESENTATION('material name',(#8333),#25061);
#8294=REPRESENTATION('density',(#8193),#25061);
#8295=REPRESENTATION('material name',(#8334),#25062);
#8296=REPRESENTATION('density',(#8194),#25062);
#8297=REPRESENTATION('material name',(#8335),#25064);
#8298=REPRESENTATION('density',(#8195),#25064);
#8299=REPRESENTATION('material name',(#8336),#25065);
#8300=REPRESENTATION('density',(#8196),#25065);
#8301=REPRESENTATION('material name',(#8337),#25066);
#8302=REPRESENTATION('density',(#8197),#25066);
#8303=REPRESENTATION('material name',(#8338),#25067);
#8304=REPRESENTATION('density',(#8198),#25067);
#8305=REPRESENTATION('material name',(#8339),#25068);
#8306=REPRESENTATION('density',(#8199),#25068);
#8307=REPRESENTATION('material name',(#8340),#25069);
#8308=REPRESENTATION('density',(#8200),#25069);
#8309=REPRESENTATION('material name',(#8341),#25070);
#8310=REPRESENTATION('density',(#8201),#25070);
#8311=REPRESENTATION('material name',(#8342),#25071);
#8312=REPRESENTATION('density',(#8202),#25071);
#8313=REPRESENTATION('material name',(#8343),#25072);
#8314=REPRESENTATION('density',(#8203),#25072);
#8315=REPRESENTATION('material name',(#8344),#25073);
#8316=REPRESENTATION('density',(#8204),#25073);
#8317=DESCRIPTIVE_REPRESENTATION_ITEM('Steel','Steel');
#8318=DESCRIPTIVE_REPRESENTATION_ITEM('Steel','Steel');
#8319=DESCRIPTIVE_REPRESENTATION_ITEM('Steel','Steel');
#8320=DESCRIPTIVE_REPRESENTATION_ITEM('Steel','Steel');
#8321=DESCRIPTIVE_REPRESENTATION_ITEM('Steel','Steel');
#8322=DESCRIPTIVE_REPRESENTATION_ITEM('Steel','Steel');
#8323=DESCRIPTIVE_REPRESENTATION_ITEM('Steel','Steel');
#8324=DESCRIPTIVE_REPRESENTATION_ITEM('Steel','Steel');
#8325=DESCRIPTIVE_REPRESENTATION_ITEM('Steel','Steel');
#8326=DESCRIPTIVE_REPRESENTATION_ITEM('Steel','Steel');
#8327=DESCRIPTIVE_REPRESENTATION_ITEM('Steel','Steel');
#8328=DESCRIPTIVE_REPRESENTATION_ITEM('Steel','Steel');
#8329=DESCRIPTIVE_REPRESENTATION_ITEM('Steel','Steel');
#8330=DESCRIPTIVE_REPRESENTATION_ITEM('Steel','Steel');
#8331=DESCRIPTIVE_REPRESENTATION_ITEM('Steel','Steel');
#8332=DESCRIPTIVE_REPRESENTATION_ITEM('Steel','Steel');
#8333=DESCRIPTIVE_REPRESENTATION_ITEM('Steel','Steel');
#8334=DESCRIPTIVE_REPRESENTATION_ITEM('Steel','Steel');
#8335=DESCRIPTIVE_REPRESENTATION_ITEM('Steel','Steel');
#8336=DESCRIPTIVE_REPRESENTATION_ITEM('Steel','Steel');
#8337=DESCRIPTIVE_REPRESENTATION_ITEM('Steel','Steel');
#8338=DESCRIPTIVE_REPRESENTATION_ITEM('Steel','Steel');
#8339=DESCRIPTIVE_REPRESENTATION_ITEM('Steel','Steel');
#8340=DESCRIPTIVE_REPRESENTATION_ITEM('Steel','Steel');
#8341=DESCRIPTIVE_REPRESENTATION_ITEM('Steel','Steel');
#8342=DESCRIPTIVE_REPRESENTATION_ITEM('Steel','Steel');
#8343=DESCRIPTIVE_REPRESENTATION_ITEM('Steel','Steel');
#8344=DESCRIPTIVE_REPRESENTATION_ITEM('Steel','Steel');
#8345=PROPERTY_DEFINITION('material property','material name',#25230);
#8346=PROPERTY_DEFINITION('material property','density of part',#25230);
#8347=PROPERTY_DEFINITION('material property','material name',#25231);
#8348=PROPERTY_DEFINITION('material property','density of part',#25231);
#8349=PROPERTY_DEFINITION('material property','material name',#25232);
#8350=PROPERTY_DEFINITION('material property','density of part',#25232);
#8351=PROPERTY_DEFINITION('material property','material name',#25233);
#8352=PROPERTY_DEFINITION('material property','density of part',#25233);
#8353=PROPERTY_DEFINITION('material property','material name',#25234);
#8354=PROPERTY_DEFINITION('material property','density of part',#25234);
#8355=PROPERTY_DEFINITION('material property','material name',#25235);
#8356=PROPERTY_DEFINITION('material property','density of part',#25235);
#8357=PROPERTY_DEFINITION('material property','material name',#25236);
#8358=PROPERTY_DEFINITION('material property','density of part',#25236);
#8359=PROPERTY_DEFINITION('material property','material name',#25238);
#8360=PROPERTY_DEFINITION('material property','density of part',#25238);
#8361=PROPERTY_DEFINITION('material property','material name',#25239);
#8362=PROPERTY_DEFINITION('material property','density of part',#25239);
#8363=PROPERTY_DEFINITION('material property','material name',#25240);
#8364=PROPERTY_DEFINITION('material property','density of part',#25240);
#8365=PROPERTY_DEFINITION('material property','material name',#25241);
#8366=PROPERTY_DEFINITION('material property','density of part',#25241);
#8367=PROPERTY_DEFINITION('material property','material name',#25242);
#8368=PROPERTY_DEFINITION('material property','density of part',#25242);
#8369=PROPERTY_DEFINITION('material property','material name',#25244);
#8370=PROPERTY_DEFINITION('material property','density of part',#25244);
#8371=PROPERTY_DEFINITION('material property','material name',#25245);
#8372=PROPERTY_DEFINITION('material property','density of part',#25245);
#8373=PROPERTY_DEFINITION('material property','material name',#25246);
#8374=PROPERTY_DEFINITION('material property','density of part',#25246);
#8375=PROPERTY_DEFINITION('material property','material name',#25247);
#8376=PROPERTY_DEFINITION('material property','density of part',#25247);
#8377=PROPERTY_DEFINITION('material property','material name',#25248);
#8378=PROPERTY_DEFINITION('material property','density of part',#25248);
#8379=PROPERTY_DEFINITION('material property','material name',#25249);
#8380=PROPERTY_DEFINITION('material property','density of part',#25249);
#8381=PROPERTY_DEFINITION('material property','material name',#25251);
#8382=PROPERTY_DEFINITION('material property','density of part',#25251);
#8383=PROPERTY_DEFINITION('material property','material name',#25252);
#8384=PROPERTY_DEFINITION('material property','density of part',#25252);
#8385=PROPERTY_DEFINITION('material property','material name',#25253);
#8386=PROPERTY_DEFINITION('material property','density of part',#25253);
#8387=PROPERTY_DEFINITION('material property','material name',#25254);
#8388=PROPERTY_DEFINITION('material property','density of part',#25254);
#8389=PROPERTY_DEFINITION('material property','material name',#25255);
#8390=PROPERTY_DEFINITION('material property','density of part',#25255);
#8391=PROPERTY_DEFINITION('material property','material name',#25256);
#8392=PROPERTY_DEFINITION('material property','density of part',#25256);
#8393=PROPERTY_DEFINITION('material property','material name',#25257);
#8394=PROPERTY_DEFINITION('material property','density of part',#25257);
#8395=PROPERTY_DEFINITION('material property','material name',#25258);
#8396=PROPERTY_DEFINITION('material property','density of part',#25258);
#8397=PROPERTY_DEFINITION('material property','material name',#25259);
#8398=PROPERTY_DEFINITION('material property','density of part',#25259);
#8399=PROPERTY_DEFINITION('material property','material name',#25260);
#8400=PROPERTY_DEFINITION('material property','density of part',#25260);
#8401=AXIS2_PLACEMENT_3D('',#11318,#9204,#9205);
#8402=AXIS2_PLACEMENT_3D('',#11319,#9206,#9207);
#8403=AXIS2_PLACEMENT_3D('',#11320,#9208,#9209);
#8404=AXIS2_PLACEMENT_3D('',#11321,#9210,#9211);
#8405=AXIS2_PLACEMENT_3D('',#11323,#9212,#9213);
#8406=AXIS2_PLACEMENT_3D('',#11326,#9215,#9216);
#8407=AXIS2_PLACEMENT_3D('',#11327,#9217,#9218);
#8408=AXIS2_PLACEMENT_3D('',#11329,#9219,#9220);
#8409=AXIS2_PLACEMENT_3D('',#11332,#9222,#9223);
#8410=AXIS2_PLACEMENT_3D('',#11333,#9224,#9225);
#8411=AXIS2_PLACEMENT_3D('',#11335,#9226,#9227);
#8412=AXIS2_PLACEMENT_3D('',#11338,#9229,#9230);
#8413=AXIS2_PLACEMENT_3D('',#11339,#9231,#9232);
#8414=AXIS2_PLACEMENT_3D('',#11341,#9233,#9234);
#8415=AXIS2_PLACEMENT_3D('',#11344,#9236,#9237);
#8416=AXIS2_PLACEMENT_3D('',#11345,#9238,#9239);
#8417=AXIS2_PLACEMENT_3D('',#11347,#9240,#9241);
#8418=AXIS2_PLACEMENT_3D('',#11350,#9243,#9244);
#8419=AXIS2_PLACEMENT_3D('',#11351,#9245,#9246);
#8420=AXIS2_PLACEMENT_3D('',#11353,#9247,#9248);
#8421=AXIS2_PLACEMENT_3D('',#11356,#9250,#9251);
#8422=AXIS2_PLACEMENT_3D('',#11357,#9252,#9253);
#8423=AXIS2_PLACEMENT_3D('',#11359,#9254,#9255);
#8424=AXIS2_PLACEMENT_3D('',#11362,#9257,#9258);
#8425=AXIS2_PLACEMENT_3D('',#11363,#9259,#9260);
#8426=AXIS2_PLACEMENT_3D('',#11372,#9265,#9266);
#8427=AXIS2_PLACEMENT_3D('',#11378,#9270,#9271);
#8428=AXIS2_PLACEMENT_3D('',#11384,#9275,#9276);
#8429=AXIS2_PLACEMENT_3D('',#11387,#9279,#9280);
#8430=AXIS2_PLACEMENT_3D('',#11388,#9281,#9282);
#8431=AXIS2_PLACEMENT_3D('',#11389,#9283,#9284);
#8432=AXIS2_PLACEMENT_3D('',#11390,#9285,#9286);
#8433=AXIS2_PLACEMENT_3D('',#11392,#9287,#9288);
#8434=AXIS2_PLACEMENT_3D('',#11395,#9290,#9291);
#8435=AXIS2_PLACEMENT_3D('',#11396,#9292,#9293);
#8436=AXIS2_PLACEMENT_3D('',#11397,#9294,#9295);
#8437=AXIS2_PLACEMENT_3D('',#11399,#9296,#9297);
#8438=AXIS2_PLACEMENT_3D('',#11402,#9299,#9300);
#8439=AXIS2_PLACEMENT_3D('',#11403,#9301,#9302);
#8440=AXIS2_PLACEMENT_3D('',#11404,#9303,#9304);
#8441=AXIS2_PLACEMENT_3D('',#11406,#9305,#9306);
#8442=AXIS2_PLACEMENT_3D('',#11409,#9308,#9309);
#8443=AXIS2_PLACEMENT_3D('',#11410,#9310,#9311);
#8444=AXIS2_PLACEMENT_3D('',#11411,#9312,#9313);
#8445=AXIS2_PLACEMENT_3D('',#11420,#9318,#9319);
#8446=AXIS2_PLACEMENT_3D('',#11426,#9323,#9324);
#8447=AXIS2_PLACEMENT_3D('',#11432,#9328,#9329);
#8448=AXIS2_PLACEMENT_3D('',#11435,#9332,#9333);
#8449=AXIS2_PLACEMENT_3D('',#11436,#9334,#9335);
#8450=AXIS2_PLACEMENT_3D('',#11437,#9336,#9337);
#8451=AXIS2_PLACEMENT_3D('',#11438,#9338,#9339);
#8452=AXIS2_PLACEMENT_3D('',#11440,#9340,#9341);
#8453=AXIS2_PLACEMENT_3D('',#11443,#9343,#9344);
#8454=AXIS2_PLACEMENT_3D('',#11444,#9345,#9346);
#8455=AXIS2_PLACEMENT_3D('',#11445,#9347,#9348);
#8456=AXIS2_PLACEMENT_3D('',#11447,#9349,#9350);
#8457=AXIS2_PLACEMENT_3D('',#11450,#9352,#9353);
#8458=AXIS2_PLACEMENT_3D('',#11451,#9354,#9355);
#8459=AXIS2_PLACEMENT_3D('',#11452,#9356,#9357);
#8460=AXIS2_PLACEMENT_3D('',#11454,#9358,#9359);
#8461=AXIS2_PLACEMENT_3D('',#11457,#9361,#9362);
#8462=AXIS2_PLACEMENT_3D('',#11458,#9363,#9364);
#8463=AXIS2_PLACEMENT_3D('',#11459,#9365,#9366);
#8464=AXIS2_PLACEMENT_3D('',#11461,#9367,#9368);
#8465=AXIS2_PLACEMENT_3D('',#11464,#9370,#9371);
#8466=AXIS2_PLACEMENT_3D('',#11465,#9372,#9373);
#8467=AXIS2_PLACEMENT_3D('',#11466,#9374,#9375);
#8468=AXIS2_PLACEMENT_3D('',#11475,#9380,#9381);
#8469=AXIS2_PLACEMENT_3D('',#11481,#9385,#9386);
#8470=AXIS2_PLACEMENT_3D('',#11487,#9390,#9391);
#8471=AXIS2_PLACEMENT_3D('',#11490,#9394,#9395);
#8472=AXIS2_PLACEMENT_3D('',#11491,#9396,#9397);
#8473=AXIS2_PLACEMENT_3D('',#11492,#9398,#9399);
#8474=AXIS2_PLACEMENT_3D('',#11493,#9400,#9401);
#8475=AXIS2_PLACEMENT_3D('',#11495,#9402,#9403);
#8476=AXIS2_PLACEMENT_3D('',#11498,#9405,#9406);
#8477=AXIS2_PLACEMENT_3D('',#11499,#9407,#9408);
#8478=AXIS2_PLACEMENT_3D('',#11501,#9409,#9410);
#8479=AXIS2_PLACEMENT_3D('',#11504,#9412,#9413);
#8480=AXIS2_PLACEMENT_3D('',#11505,#9414,#9415);
#8481=AXIS2_PLACEMENT_3D('',#11507,#9416,#9417);
#8482=AXIS2_PLACEMENT_3D('',#11510,#9419,#9420);
#8483=AXIS2_PLACEMENT_3D('',#11511,#9421,#9422);
#8484=AXIS2_PLACEMENT_3D('',#11513,#9423,#9424);
#8485=AXIS2_PLACEMENT_3D('',#11516,#9426,#9427);
#8486=AXIS2_PLACEMENT_3D('',#11517,#9428,#9429);
#8487=AXIS2_PLACEMENT_3D('',#11519,#9430,#9431);
#8488=AXIS2_PLACEMENT_3D('',#11520,#9432,#9433);
#8489=AXIS2_PLACEMENT_3D('',#11522,#9434,#9435);
#8490=AXIS2_PLACEMENT_3D('',#11524,#9437,#9438);
#8491=AXIS2_PLACEMENT_3D('',#11526,#9439,#9440);
#8492=AXIS2_PLACEMENT_3D('',#11529,#9442,#9443);
#8493=AXIS2_PLACEMENT_3D('',#11530,#9444,#9445);
#8494=AXIS2_PLACEMENT_3D('',#11531,#9446,#9447);
#8495=AXIS2_PLACEMENT_3D('',#11533,#9448,#9449);
#8496=AXIS2_PLACEMENT_3D('',#11536,#9451,#9452);
#8497=AXIS2_PLACEMENT_3D('',#11537,#9453,#9454);
#8498=AXIS2_PLACEMENT_3D('',#11538,#9455,#9456);
#8499=AXIS2_PLACEMENT_3D('',#11547,#9461,#9462);
#8500=AXIS2_PLACEMENT_3D('',#11553,#9466,#9467);
#8501=AXIS2_PLACEMENT_3D('',#11559,#9471,#9472);
#8502=AXIS2_PLACEMENT_3D('',#11562,#9475,#9476);
#8503=AXIS2_PLACEMENT_3D('',#11563,#9477,#9478);
#8504=AXIS2_PLACEMENT_3D('',#11564,#9479,#9480);
#8505=AXIS2_PLACEMENT_3D('',#11565,#9481,#9482);
#8506=AXIS2_PLACEMENT_3D('',#11567,#9483,#9484);
#8507=AXIS2_PLACEMENT_3D('',#11570,#9486,#9487);
#8508=AXIS2_PLACEMENT_3D('',#11571,#9488,#9489);
#8509=AXIS2_PLACEMENT_3D('',#11573,#9490,#9491);
#8510=AXIS2_PLACEMENT_3D('',#11576,#9493,#9494);
#8511=AXIS2_PLACEMENT_3D('',#11577,#9495,#9496);
#8512=AXIS2_PLACEMENT_3D('',#11579,#9497,#9498);
#8513=AXIS2_PLACEMENT_3D('',#11582,#9500,#9501);
#8514=AXIS2_PLACEMENT_3D('',#11583,#9502,#9503);
#8515=AXIS2_PLACEMENT_3D('',#11592,#9508,#9509);
#8516=AXIS2_PLACEMENT_3D('',#11593,#9510,#9511);
#8517=AXIS2_PLACEMENT_3D('',#11595,#9512,#9513);
#8518=AXIS2_PLACEMENT_3D('',#11596,#9514,#9515);
#8519=AXIS2_PLACEMENT_3D('',#11597,#9516,#9517);
#8520=AXIS2_PLACEMENT_3D('',#11598,#9518,#9519);
#8521=AXIS2_PLACEMENT_3D('',#11601,#9521,#9522);
#8522=AXIS2_PLACEMENT_3D('',#11602,#9523,#9524);
#8523=AXIS2_PLACEMENT_3D('',#11604,#9525,#9526);
#8524=AXIS2_PLACEMENT_3D('',#11605,#9527,#9528);
#8525=AXIS2_PLACEMENT_3D('',#11607,#9529,#9530);
#8526=AXIS2_PLACEMENT_3D('',#11609,#9532,#9533);
#8527=AXIS2_PLACEMENT_3D('',#11610,#9534,#9535);
#8528=AXIS2_PLACEMENT_3D('',#11611,#9536,#9537);
#8529=AXIS2_PLACEMENT_3D('',#11620,#9542,#9543);
#8530=AXIS2_PLACEMENT_3D('',#11627,#9547,#9548);
#8531=AXIS2_PLACEMENT_3D('',#11629,#9549,#9550);
#8532=AXIS2_PLACEMENT_3D('',#11630,#9551,#9552);
#8533=AXIS2_PLACEMENT_3D('',#11634,#9555,#9556);
#8534=AXIS2_PLACEMENT_3D('',#11638,#9559,#9560);
#8535=AXIS2_PLACEMENT_3D('',#11641,#9562,#9563);
#8536=AXIS2_PLACEMENT_3D('',#11643,#9564,#9565);
#8537=AXIS2_PLACEMENT_3D('',#11644,#9566,#9567);
#8538=AXIS2_PLACEMENT_3D('',#11646,#9568,#9569);
#8539=AXIS2_PLACEMENT_3D('',#11648,#9571,#9572);
#8540=AXIS2_PLACEMENT_3D('',#11650,#9573,#9574);
#8541=AXIS2_PLACEMENT_3D('',#11651,#9575,#9576);
#8542=AXIS2_PLACEMENT_3D('',#11653,#9577,#9578);
#8543=AXIS2_PLACEMENT_3D('',#11655,#9580,#9581);
#8544=AXIS2_PLACEMENT_3D('',#11657,#9582,#9583);
#8545=AXIS2_PLACEMENT_3D('',#11658,#9584,#9585);
#8546=AXIS2_PLACEMENT_3D('',#11660,#9587,#9588);
#8547=AXIS2_PLACEMENT_3D('',#11662,#9590,#9591);
#8548=AXIS2_PLACEMENT_3D('',#11663,#9592,#9593);
#8549=AXIS2_PLACEMENT_3D('',#11664,#9594,#9595);
#8550=AXIS2_PLACEMENT_3D('',#11673,#9600,#9601);
#8551=AXIS2_PLACEMENT_3D('',#11679,#9605,#9606);
#8552=AXIS2_PLACEMENT_3D('',#11685,#9610,#9611);
#8553=AXIS2_PLACEMENT_3D('',#11691,#9615,#9616);
#8554=AXIS2_PLACEMENT_3D('',#11697,#9620,#9621);
#8555=AXIS2_PLACEMENT_3D('',#11700,#9624,#9625);
#8556=AXIS2_PLACEMENT_3D('',#11701,#9626,#9627);
#8557=AXIS2_PLACEMENT_3D('',#11702,#9628,#9629);
#8558=AXIS2_PLACEMENT_3D('',#11704,#9630,#9631);
#8559=AXIS2_PLACEMENT_3D('',#11705,#9632,#9633);
#8560=AXIS2_PLACEMENT_3D('',#11707,#9634,#9635);
#8561=AXIS2_PLACEMENT_3D('',#11708,#9636,#9637);
#8562=AXIS2_PLACEMENT_3D('',#11710,#9638,#9639);
#8563=AXIS2_PLACEMENT_3D('',#11712,#9641,#9642);
#8564=AXIS2_PLACEMENT_3D('',#11714,#9643,#9644);
#8565=AXIS2_PLACEMENT_3D('',#11716,#9646,#9647);
#8566=AXIS2_PLACEMENT_3D('',#11718,#9648,#9649);
#8567=AXIS2_PLACEMENT_3D('',#11720,#9651,#9652);
#8568=AXIS2_PLACEMENT_3D('',#11722,#9653,#9654);
#8569=AXIS2_PLACEMENT_3D('',#11723,#9655,#9656);
#8570=AXIS2_PLACEMENT_3D('',#11725,#9657,#9658);
#8571=AXIS2_PLACEMENT_3D('',#11727,#9660,#9661);
#8572=AXIS2_PLACEMENT_3D('',#11729,#9663,#9664);
#8573=AXIS2_PLACEMENT_3D('',#11730,#9665,#9666);
#8574=AXIS2_PLACEMENT_3D('',#11731,#9667,#9668);
#8575=AXIS2_PLACEMENT_3D('',#11734,#9669,#9670);
#8576=AXIS2_PLACEMENT_3D('',#11735,#9671,#9672);
#8577=AXIS2_PLACEMENT_3D('',#11737,#9673,#9674);
#8578=AXIS2_PLACEMENT_3D('',#11739,#9675,#9676);
#8579=AXIS2_PLACEMENT_3D('',#11740,#9677,#9678);
#8580=AXIS2_PLACEMENT_3D('',#11741,#9679,#9680);
#8581=AXIS2_PLACEMENT_3D('',#11744,#9682,#9683);
#8582=AXIS2_PLACEMENT_3D('',#11745,#9684,#9685);
#8583=AXIS2_PLACEMENT_3D('',#11747,#9686,#9687);
#8584=AXIS2_PLACEMENT_3D('',#11750,#9689,#9690);
#8585=AXIS2_PLACEMENT_3D('',#11751,#9691,#9692);
#8586=AXIS2_PLACEMENT_3D('',#11754,#9694,#9695);
#8587=AXIS2_PLACEMENT_3D('',#11755,#9696,#9697);
#8588=AXIS2_PLACEMENT_3D('',#11756,#9698,#9699);
#8589=AXIS2_PLACEMENT_3D('',#11758,#9700,#9701);
#8590=AXIS2_PLACEMENT_3D('',#11760,#9703,#9704);
#8591=AXIS2_PLACEMENT_3D('',#11762,#9705,#9706);
#8592=AXIS2_PLACEMENT_3D('',#11763,#9707,#9708);
#8593=AXIS2_PLACEMENT_3D('',#11765,#9710,#9711);
#8594=AXIS2_PLACEMENT_3D('',#11766,#9712,#9713);
#8595=AXIS2_PLACEMENT_3D('',#11769,#9714,#9715);
#8596=AXIS2_PLACEMENT_3D('',#11770,#9716,#9717);
#8597=AXIS2_PLACEMENT_3D('',#11772,#9718,#9719);
#8598=AXIS2_PLACEMENT_3D('',#11774,#9720,#9721);
#8599=AXIS2_PLACEMENT_3D('',#11775,#9722,#9723);
#8600=AXIS2_PLACEMENT_3D('',#11776,#9724,#9725);
#8601=AXIS2_PLACEMENT_3D('',#11778,#9726,#9727);
#8602=AXIS2_PLACEMENT_3D('',#11780,#9729,#9730);
#8603=AXIS2_PLACEMENT_3D('',#11782,#9731,#9732);
#8604=AXIS2_PLACEMENT_3D('',#11784,#9733,#9734);
#8605=AXIS2_PLACEMENT_3D('',#11785,#9735,#9736);
#8606=AXIS2_PLACEMENT_3D('',#11787,#9737,#9738);
#8607=AXIS2_PLACEMENT_3D('',#11789,#9740,#9741);
#8608=AXIS2_PLACEMENT_3D('',#11791,#9742,#9743);
#8609=AXIS2_PLACEMENT_3D('',#11793,#9745,#9746);
#8610=AXIS2_PLACEMENT_3D('',#11795,#9747,#9748);
#8611=AXIS2_PLACEMENT_3D('',#11797,#9750,#9751);
#8612=AXIS2_PLACEMENT_3D('',#11798,#9752,#9753);
#8613=AXIS2_PLACEMENT_3D('',#11800,#9755,#9756);
#8614=AXIS2_PLACEMENT_3D('',#11801,#9757,#9758);
#8615=AXIS2_PLACEMENT_3D('',#11804,#9759,#9760);
#8616=AXIS2_PLACEMENT_3D('',#11805,#9761,#9762);
#8617=AXIS2_PLACEMENT_3D('',#11808,#9763,#9764);
#8618=AXIS2_PLACEMENT_3D('',#11809,#9765,#9766);
#8619=AXIS2_PLACEMENT_3D('',#11812,#9767,#9768);
#8620=AXIS2_PLACEMENT_3D('',#11813,#9769,#9770);
#8621=AXIS2_PLACEMENT_3D('',#11816,#9771,#9772);
#8622=AXIS2_PLACEMENT_3D('',#11817,#9773,#9774);
#8623=AXIS2_PLACEMENT_3D('',#11820,#9775,#9776);
#8624=AXIS2_PLACEMENT_3D('',#11821,#9777,#9778);
#8625=AXIS2_PLACEMENT_3D('',#11824,#9779,#9780);
#8626=AXIS2_PLACEMENT_3D('',#11825,#9781,#9782);
#8627=AXIS2_PLACEMENT_3D('',#11828,#9783,#9784);
#8628=AXIS2_PLACEMENT_3D('',#11829,#9785,#9786);
#8629=AXIS2_PLACEMENT_3D('',#11832,#9787,#9788);
#8630=AXIS2_PLACEMENT_3D('',#11833,#9789,#9790);
#8631=AXIS2_PLACEMENT_3D('',#11834,#9791,#9792);
#8632=AXIS2_PLACEMENT_3D('',#11860,#9793,#9794);
#8633=AXIS2_PLACEMENT_3D('',#11884,#9795,#9796);
#8634=AXIS2_PLACEMENT_3D('',#11885,#9797,#9798);
#8635=AXIS2_PLACEMENT_3D('',#11887,#9799,#9800);
#8636=AXIS2_PLACEMENT_3D('',#11912,#9801,#9802);
#8637=AXIS2_PLACEMENT_3D('',#11937,#9803,#9804);
#8638=AXIS2_PLACEMENT_3D('',#11953,#9806,#9807);
#8639=AXIS2_PLACEMENT_3D('',#11968,#9808,#9809);
#8640=AXIS2_PLACEMENT_3D('',#11993,#9810,#9811);
#8641=AXIS2_PLACEMENT_3D('',#12018,#9812,#9813);
#8642=AXIS2_PLACEMENT_3D('',#12043,#9814,#9815);
#8643=AXIS2_PLACEMENT_3D('',#12067,#9816,#9817);
#8644=AXIS2_PLACEMENT_3D('',#12068,#9818,#9819);
#8645=AXIS2_PLACEMENT_3D('',#12070,#9820,#9821);
#8646=AXIS2_PLACEMENT_3D('',#12071,#9822,#9823);
#8647=AXIS2_PLACEMENT_3D('',#12072,#9824,#9825);
#8648=AXIS2_PLACEMENT_3D('',#12096,#9826,#9827);
#8649=AXIS2_PLACEMENT_3D('',#12097,#9828,#9829);
#8650=AXIS2_PLACEMENT_3D('',#12099,#9830,#9831);
#8651=AXIS2_PLACEMENT_3D('',#12100,#9832,#9833);
#8652=AXIS2_PLACEMENT_3D('',#12101,#9834,#9835);
#8653=AXIS2_PLACEMENT_3D('',#12125,#9836,#9837);
#8654=AXIS2_PLACEMENT_3D('',#12126,#9838,#9839);
#8655=AXIS2_PLACEMENT_3D('',#12128,#9840,#9841);
#8656=AXIS2_PLACEMENT_3D('',#12129,#9842,#9843);
#8657=AXIS2_PLACEMENT_3D('',#12130,#9844,#9845);
#8658=AXIS2_PLACEMENT_3D('',#12145,#9846,#9847);
#8659=AXIS2_PLACEMENT_3D('',#12158,#9848,#9849);
#8660=AXIS2_PLACEMENT_3D('',#12160,#9850,#9851);
#8661=AXIS2_PLACEMENT_3D('',#12161,#9852,#9853);
#8662=AXIS2_PLACEMENT_3D('',#12162,#9854,#9855);
#8663=AXIS2_PLACEMENT_3D('',#12186,#9856,#9857);
#8664=AXIS2_PLACEMENT_3D('',#12187,#9858,#9859);
#8665=AXIS2_PLACEMENT_3D('',#12189,#9860,#9861);
#8666=AXIS2_PLACEMENT_3D('',#12190,#9862,#9863);
#8667=AXIS2_PLACEMENT_3D('',#12191,#9864,#9865);
#8668=AXIS2_PLACEMENT_3D('',#12215,#9866,#9867);
#8669=AXIS2_PLACEMENT_3D('',#12216,#9868,#9869);
#8670=AXIS2_PLACEMENT_3D('',#12218,#9870,#9871);
#8671=AXIS2_PLACEMENT_3D('',#12219,#9872,#9873);
#8672=AXIS2_PLACEMENT_3D('',#12220,#9874,#9875);
#8673=AXIS2_PLACEMENT_3D('',#12244,#9876,#9877);
#8674=AXIS2_PLACEMENT_3D('',#12245,#9878,#9879);
#8675=AXIS2_PLACEMENT_3D('',#12247,#9880,#9881);
#8676=AXIS2_PLACEMENT_3D('',#12250,#9883,#9884);
#8677=AXIS2_PLACEMENT_3D('',#12274,#9885,#9886);
#8678=AXIS2_PLACEMENT_3D('',#12275,#9887,#9888);
#8679=AXIS2_PLACEMENT_3D('',#12276,#9889,#9890);
#8680=AXIS2_PLACEMENT_3D('',#12277,#9891,#9892);
#8681=AXIS2_PLACEMENT_3D('',#12278,#9893,#9894);
#8682=AXIS2_PLACEMENT_3D('',#12279,#9895,#9896);
#8683=AXIS2_PLACEMENT_3D('',#12280,#9897,#9898);
#8684=AXIS2_PLACEMENT_3D('',#12281,#9899,#9900);
#8685=AXIS2_PLACEMENT_3D('',#12282,#9901,#9902);
#8686=AXIS2_PLACEMENT_3D('',#12284,#9903,#9904);
#8687=AXIS2_PLACEMENT_3D('',#12286,#9905,#9906);
#8688=AXIS2_PLACEMENT_3D('',#12287,#9907,#9908);
#8689=AXIS2_PLACEMENT_3D('',#12289,#9909,#9910);
#8690=AXIS2_PLACEMENT_3D('',#12291,#9912,#9913);
#8691=AXIS2_PLACEMENT_3D('',#12293,#9914,#9915);
#8692=AXIS2_PLACEMENT_3D('',#12294,#9916,#9917);
#8693=AXIS2_PLACEMENT_3D('',#12296,#9919,#9920);
#8694=AXIS2_PLACEMENT_3D('',#12298,#9921,#9922);
#8695=AXIS2_PLACEMENT_3D('',#12300,#9923,#9924);
#8696=AXIS2_PLACEMENT_3D('',#12301,#9925,#9926);
#8697=AXIS2_PLACEMENT_3D('',#12303,#9927,#9928);
#8698=AXIS2_PLACEMENT_3D('',#12305,#9930,#9931);
#8699=AXIS2_PLACEMENT_3D('',#12307,#9932,#9933);
#8700=AXIS2_PLACEMENT_3D('',#12308,#9934,#9935);
#8701=AXIS2_PLACEMENT_3D('',#12310,#9937,#9938);
#8702=AXIS2_PLACEMENT_3D('',#12311,#9939,#9940);
#8703=AXIS2_PLACEMENT_3D('',#12312,#9941,#9942);
#8704=AXIS2_PLACEMENT_3D('',#12313,#9943,#9944);
#8705=AXIS2_PLACEMENT_3D('',#12314,#9945,#9946);
#8706=AXIS2_PLACEMENT_3D('',#12315,#9947,#9948);
#8707=AXIS2_PLACEMENT_3D('',#12316,#9949,#9950);
#8708=AXIS2_PLACEMENT_3D('',#12317,#9951,#9952);
#8709=AXIS2_PLACEMENT_3D('',#12319,#9953,#9954);
#8710=AXIS2_PLACEMENT_3D('',#12322,#9956,#9957);
#8711=AXIS2_PLACEMENT_3D('',#12323,#9958,#9959);
#8712=AXIS2_PLACEMENT_3D('',#12324,#9960,#9961);
#8713=AXIS2_PLACEMENT_3D('',#12326,#9962,#9963);
#8714=AXIS2_PLACEMENT_3D('',#12329,#9965,#9966);
#8715=AXIS2_PLACEMENT_3D('',#12330,#9967,#9968);
#8716=AXIS2_PLACEMENT_3D('',#12331,#9969,#9970);
#8717=AXIS2_PLACEMENT_3D('',#12333,#9971,#9972);
#8718=AXIS2_PLACEMENT_3D('',#12336,#9974,#9975);
#8719=AXIS2_PLACEMENT_3D('',#12337,#9976,#9977);
#8720=AXIS2_PLACEMENT_3D('',#12338,#9978,#9979);
#8721=AXIS2_PLACEMENT_3D('',#12340,#9980,#9981);
#8722=AXIS2_PLACEMENT_3D('',#12343,#9983,#9984);
#8723=AXIS2_PLACEMENT_3D('',#12344,#9985,#9986);
#8724=AXIS2_PLACEMENT_3D('',#12345,#9987,#9988);
#8725=AXIS2_PLACEMENT_3D('',#12347,#9989,#9990);
#8726=AXIS2_PLACEMENT_3D('',#12350,#9992,#9993);
#8727=AXIS2_PLACEMENT_3D('',#12351,#9994,#9995);
#8728=AXIS2_PLACEMENT_3D('',#12352,#9996,#9997);
#8729=AXIS2_PLACEMENT_3D('',#12354,#9998,#9999);
#8730=AXIS2_PLACEMENT_3D('',#12357,#10001,#10002);
#8731=AXIS2_PLACEMENT_3D('',#12358,#10003,#10004);
#8732=AXIS2_PLACEMENT_3D('',#12360,#10005,#10006);
#8733=AXIS2_PLACEMENT_3D('',#12361,#10007,#10008);
#8734=AXIS2_PLACEMENT_3D('',#12363,#10009,#10010);
#8735=AXIS2_PLACEMENT_3D('',#12365,#10012,#10013);
#8736=AXIS2_PLACEMENT_3D('',#12367,#10014,#10015);
#8737=AXIS2_PLACEMENT_3D('',#12370,#10017,#10018);
#8738=AXIS2_PLACEMENT_3D('',#12371,#10019,#10020);
#8739=AXIS2_PLACEMENT_3D('',#12373,#10021,#10022);
#8740=AXIS2_PLACEMENT_3D('',#12374,#10023,#10024);
#8741=AXIS2_PLACEMENT_3D('',#12376,#10025,#10026);
#8742=AXIS2_PLACEMENT_3D('',#12378,#10028,#10029);
#8743=AXIS2_PLACEMENT_3D('',#12380,#10030,#10031);
#8744=AXIS2_PLACEMENT_3D('',#12383,#10033,#10034);
#8745=AXIS2_PLACEMENT_3D('',#12384,#10035,#10036);
#8746=AXIS2_PLACEMENT_3D('',#12393,#10041,#10042);
#8747=AXIS2_PLACEMENT_3D('',#12399,#10046,#10047);
#8748=AXIS2_PLACEMENT_3D('',#12405,#10051,#10052);
#8749=AXIS2_PLACEMENT_3D('',#12415,#10058,#10059);
#8750=AXIS2_PLACEMENT_3D('',#12419,#10062,#10063);
#8751=AXIS2_PLACEMENT_3D('',#12423,#10066,#10067);
#8752=AXIS2_PLACEMENT_3D('',#12429,#10071,#10072);
#8753=AXIS2_PLACEMENT_3D('',#12432,#10075,#10076);
#8754=AXIS2_PLACEMENT_3D('',#12433,#10077,#10078);
#8755=AXIS2_PLACEMENT_3D('',#12434,#10079,#10080);
#8756=AXIS2_PLACEMENT_3D('',#12435,#10081,#10082);
#8757=AXIS2_PLACEMENT_3D('',#12444,#10087,#10088);
#8758=AXIS2_PLACEMENT_3D('',#12450,#10092,#10093);
#8759=AXIS2_PLACEMENT_3D('',#12456,#10097,#10098);
#8760=AXIS2_PLACEMENT_3D('',#12459,#10101,#10102);
#8761=AXIS2_PLACEMENT_3D('',#12460,#10103,#10104);
#8762=AXIS2_PLACEMENT_3D('',#12461,#10105,#10106);
#8763=AXIS2_PLACEMENT_3D('',#12462,#10107,#10108);
#8764=AXIS2_PLACEMENT_3D('',#12471,#10113,#10114);
#8765=AXIS2_PLACEMENT_3D('',#12478,#10118,#10119);
#8766=AXIS2_PLACEMENT_3D('',#12480,#10120,#10121);
#8767=AXIS2_PLACEMENT_3D('',#12481,#10122,#10123);
#8768=AXIS2_PLACEMENT_3D('',#12485,#10126,#10127);
#8769=AXIS2_PLACEMENT_3D('',#12489,#10130,#10131);
#8770=AXIS2_PLACEMENT_3D('',#12492,#10133,#10134);
#8771=AXIS2_PLACEMENT_3D('',#12494,#10135,#10136);
#8772=AXIS2_PLACEMENT_3D('',#12495,#10137,#10138);
#8773=AXIS2_PLACEMENT_3D('',#12498,#10140,#10141);
#8774=AXIS2_PLACEMENT_3D('',#12499,#10142,#10143);
#8775=AXIS2_PLACEMENT_3D('',#12501,#10144,#10145);
#8776=AXIS2_PLACEMENT_3D('',#12502,#10146,#10147);
#8777=AXIS2_PLACEMENT_3D('',#12505,#10149,#10150);
#8778=AXIS2_PLACEMENT_3D('',#12506,#10151,#10152);
#8779=AXIS2_PLACEMENT_3D('',#12508,#10153,#10154);
#8780=AXIS2_PLACEMENT_3D('',#12509,#10155,#10156);
#8781=AXIS2_PLACEMENT_3D('',#12511,#10158,#10159);
#8782=AXIS2_PLACEMENT_3D('',#12513,#10161,#10162);
#8783=AXIS2_PLACEMENT_3D('',#12514,#10163,#10164);
#8784=AXIS2_PLACEMENT_3D('',#12515,#10165,#10166);
#8785=AXIS2_PLACEMENT_3D('',#12546,#10168,#10169);
#8786=AXIS2_PLACEMENT_3D('',#12587,#10170,#10171);
#8787=AXIS2_PLACEMENT_3D('',#12674,#10173,#10174);
#8788=AXIS2_PLACEMENT_3D('',#12764,#10176,#10177);
#8789=AXIS2_PLACEMENT_3D('',#12851,#10179,#10180);
#8790=AXIS2_PLACEMENT_3D('',#12941,#10182,#10183);
#8791=AXIS2_PLACEMENT_3D('',#13028,#10185,#10186);
#8792=AXIS2_PLACEMENT_3D('',#13115,#10188,#10189);
#8793=AXIS2_PLACEMENT_3D('',#13205,#10191,#10192);
#8794=AXIS2_PLACEMENT_3D('',#13210,#10194,#10195);
#8795=AXIS2_PLACEMENT_3D('',#13221,#10196,#10197);
#8796=AXIS2_PLACEMENT_3D('',#13234,#10199,#10200);
#8797=AXIS2_PLACEMENT_3D('',#13247,#10201,#10202);
#8798=AXIS2_PLACEMENT_3D('',#13284,#10204,#10205);
#8799=AXIS2_PLACEMENT_3D('',#13321,#10207,#10208);
#8800=AXIS2_PLACEMENT_3D('',#13359,#10210,#10211);
#8801=AXIS2_PLACEMENT_3D('',#13396,#10213,#10214);
#8802=AXIS2_PLACEMENT_3D('',#13433,#10216,#10217);
#8803=AXIS2_PLACEMENT_3D('',#13471,#10219,#10220);
#8804=AXIS2_PLACEMENT_3D('',#13509,#10222,#10223);
#8805=AXIS2_PLACEMENT_3D('',#13520,#10225,#10226);
#8806=AXIS2_PLACEMENT_3D('',#13531,#10227,#10228);
#8807=AXIS2_PLACEMENT_3D('',#14674,#10229,#10230);
#8808=AXIS2_PLACEMENT_3D('',#14678,#10232,#10233);
#8809=AXIS2_PLACEMENT_3D('',#14679,#10234,#10235);
#8810=AXIS2_PLACEMENT_3D('',#14681,#10236,#10237);
#8811=AXIS2_PLACEMENT_3D('',#14683,#10238,#10239);
#8812=AXIS2_PLACEMENT_3D('',#14685,#10240,#10241);
#8813=AXIS2_PLACEMENT_3D('',#14686,#10242,#10243);
#8814=AXIS2_PLACEMENT_3D('',#14688,#10244,#10245);
#8815=AXIS2_PLACEMENT_3D('',#14690,#10247,#10248);
#8816=AXIS2_PLACEMENT_3D('',#14692,#10249,#10250);
#8817=AXIS2_PLACEMENT_3D('',#14694,#10252,#10253);
#8818=AXIS2_PLACEMENT_3D('',#14696,#10254,#10255);
#8819=AXIS2_PLACEMENT_3D('',#14698,#10257,#10258);
#8820=AXIS2_PLACEMENT_3D('',#14704,#10262,#10263);
#8821=AXIS2_PLACEMENT_3D('',#14705,#10264,#10265);
#8822=AXIS2_PLACEMENT_3D('',#14707,#10266,#10267);
#8823=AXIS2_PLACEMENT_3D('',#14708,#10268,#10269);
#8824=AXIS2_PLACEMENT_3D('',#14709,#10270,#10271);
#8825=AXIS2_PLACEMENT_3D('',#14710,#10272,#10273);
#8826=AXIS2_PLACEMENT_3D('',#14713,#10275,#10276);
#8827=AXIS2_PLACEMENT_3D('',#14714,#10277,#10278);
#8828=AXIS2_PLACEMENT_3D('',#14715,#10279,#10280);
#8829=AXIS2_PLACEMENT_3D('',#14716,#10281,#10282);
#8830=AXIS2_PLACEMENT_3D('',#14718,#10283,#10284);
#8831=AXIS2_PLACEMENT_3D('',#14719,#10285,#10286);
#8832=AXIS2_PLACEMENT_3D('',#14721,#10287,#10288);
#8833=AXIS2_PLACEMENT_3D('',#14723,#10290,#10291);
#8834=AXIS2_PLACEMENT_3D('',#14725,#10292,#10293);
#8835=AXIS2_PLACEMENT_3D('',#14727,#10295,#10296);
#8836=AXIS2_PLACEMENT_3D('',#14729,#10297,#10298);
#8837=AXIS2_PLACEMENT_3D('',#14731,#10300,#10301);
#8838=AXIS2_PLACEMENT_3D('',#14733,#10302,#10303);
#8839=AXIS2_PLACEMENT_3D('',#14734,#10304,#10305);
#8840=AXIS2_PLACEMENT_3D('',#14736,#10306,#10307);
#8841=AXIS2_PLACEMENT_3D('',#14738,#10309,#10310);
#8842=AXIS2_PLACEMENT_3D('',#14740,#10311,#10312);
#8843=AXIS2_PLACEMENT_3D('',#14742,#10314,#10315);
#8844=AXIS2_PLACEMENT_3D('',#14744,#10316,#10317);
#8845=AXIS2_PLACEMENT_3D('',#14746,#10319,#10320);
#8846=AXIS2_PLACEMENT_3D('',#14747,#10321,#10322);
#8847=AXIS2_PLACEMENT_3D('',#14756,#10327,#10328);
#8848=AXIS2_PLACEMENT_3D('',#14762,#10332,#10333);
#8849=AXIS2_PLACEMENT_3D('',#14768,#10337,#10338);
#8850=AXIS2_PLACEMENT_3D('',#14774,#10342,#10343);
#8851=AXIS2_PLACEMENT_3D('',#14780,#10347,#10348);
#8852=AXIS2_PLACEMENT_3D('',#14783,#10351,#10352);
#8853=AXIS2_PLACEMENT_3D('',#14784,#10353,#10354);
#8854=AXIS2_PLACEMENT_3D('',#14785,#10355,#10356);
#8855=AXIS2_PLACEMENT_3D('',#14786,#10357,#10358);
#8856=AXIS2_PLACEMENT_3D('',#14788,#10359,#10360);
#8857=AXIS2_PLACEMENT_3D('',#14789,#10361,#10362);
#8858=AXIS2_PLACEMENT_3D('',#14791,#10363,#10364);
#8859=AXIS2_PLACEMENT_3D('',#14793,#10366,#10367);
#8860=AXIS2_PLACEMENT_3D('',#14795,#10368,#10369);
#8861=AXIS2_PLACEMENT_3D('',#14797,#10371,#10372);
#8862=AXIS2_PLACEMENT_3D('',#14799,#10373,#10374);
#8863=AXIS2_PLACEMENT_3D('',#14801,#10376,#10377);
#8864=AXIS2_PLACEMENT_3D('',#14803,#10378,#10379);
#8865=AXIS2_PLACEMENT_3D('',#14804,#10380,#10381);
#8866=AXIS2_PLACEMENT_3D('',#14806,#10382,#10383);
#8867=AXIS2_PLACEMENT_3D('',#14808,#10385,#10386);
#8868=AXIS2_PLACEMENT_3D('',#14810,#10387,#10388);
#8869=AXIS2_PLACEMENT_3D('',#14812,#10390,#10391);
#8870=AXIS2_PLACEMENT_3D('',#14814,#10392,#10393);
#8871=AXIS2_PLACEMENT_3D('',#14816,#10395,#10396);
#8872=AXIS2_PLACEMENT_3D('',#14817,#10397,#10398);
#8873=AXIS2_PLACEMENT_3D('',#14826,#10403,#10404);
#8874=AXIS2_PLACEMENT_3D('',#14832,#10408,#10409);
#8875=AXIS2_PLACEMENT_3D('',#14838,#10413,#10414);
#8876=AXIS2_PLACEMENT_3D('',#14844,#10418,#10419);
#8877=AXIS2_PLACEMENT_3D('',#14850,#10423,#10424);
#8878=AXIS2_PLACEMENT_3D('',#14853,#10427,#10428);
#8879=AXIS2_PLACEMENT_3D('',#14854,#10429,#10430);
#8880=AXIS2_PLACEMENT_3D('',#14855,#10431,#10432);
#8881=AXIS2_PLACEMENT_3D('',#14856,#10433,#10434);
#8882=AXIS2_PLACEMENT_3D('',#14857,#10435,#10436);
#8883=AXIS2_PLACEMENT_3D('',#14858,#10437,#10438);
#8884=AXIS2_PLACEMENT_3D('',#14859,#10439,#10440);
#8885=AXIS2_PLACEMENT_3D('',#14860,#10441,#10442);
#8886=AXIS2_PLACEMENT_3D('',#14861,#10443,#10444);
#8887=AXIS2_PLACEMENT_3D('',#14862,#10445,#10446);
#8888=AXIS2_PLACEMENT_3D('',#14863,#10447,#10448);
#8889=AXIS2_PLACEMENT_3D('',#14864,#10449,#10450);
#8890=AXIS2_PLACEMENT_3D('',#14865,#10451,#10452);
#8891=AXIS2_PLACEMENT_3D('',#14866,#10453,#10454);
#8892=AXIS2_PLACEMENT_3D('',#14867,#10455,#10456);
#8893=AXIS2_PLACEMENT_3D('',#14868,#10457,#10458);
#8894=AXIS2_PLACEMENT_3D('',#14893,#10460,#10461);
#8895=AXIS2_PLACEMENT_3D('',#14898,#10462,#10463);
#8896=AXIS2_PLACEMENT_3D('',#14985,#10465,#10466);
#8897=AXIS2_PLACEMENT_3D('',#15075,#10468,#10469);
#8898=AXIS2_PLACEMENT_3D('',#15162,#10471,#10472);
#8899=AXIS2_PLACEMENT_3D('',#15249,#10474,#10475);
#8900=AXIS2_PLACEMENT_3D('',#15336,#10477,#10478);
#8901=AXIS2_PLACEMENT_3D('',#15423,#10480,#10481);
#8902=AXIS2_PLACEMENT_3D('',#15510,#10483,#10484);
#8903=AXIS2_PLACEMENT_3D('',#15582,#10486,#10487);
#8904=AXIS2_PLACEMENT_3D('',#15633,#10489,#10490);
#8905=AXIS2_PLACEMENT_3D('',#15681,#10492,#10493);
#8906=AXIS2_PLACEMENT_3D('',#15729,#10495,#10496);
#8907=AXIS2_PLACEMENT_3D('',#15780,#10498,#10499);
#8908=AXIS2_PLACEMENT_3D('',#15831,#10501,#10502);
#8909=AXIS2_PLACEMENT_3D('',#15879,#10504,#10505);
#8910=AXIS2_PLACEMENT_3D('',#15930,#10507,#10508);
#8911=AXIS2_PLACEMENT_3D('',#15981,#10510,#10511);
#8912=AXIS2_PLACEMENT_3D('',#16029,#10513,#10514);
#8913=AXIS2_PLACEMENT_3D('',#16077,#10516,#10517);
#8914=AXIS2_PLACEMENT_3D('',#16128,#10519,#10520);
#8915=AXIS2_PLACEMENT_3D('',#16179,#10522,#10523);
#8916=AXIS2_PLACEMENT_3D('',#16227,#10525,#10526);
#8917=AXIS2_PLACEMENT_3D('',#16278,#10528,#10529);
#8918=AXIS2_PLACEMENT_3D('',#16329,#10531,#10532);
#8919=AXIS2_PLACEMENT_3D('',#16377,#10534,#10535);
#8920=AXIS2_PLACEMENT_3D('',#16425,#10537,#10538);
#8921=AXIS2_PLACEMENT_3D('',#16476,#10540,#10541);
#8922=AXIS2_PLACEMENT_3D('',#16527,#10543,#10544);
#8923=AXIS2_PLACEMENT_3D('',#16575,#10546,#10547);
#8924=AXIS2_PLACEMENT_3D('',#16626,#10549,#10550);
#8925=AXIS2_PLACEMENT_3D('',#16677,#10552,#10553);
#8926=AXIS2_PLACEMENT_3D('',#16725,#10555,#10556);
#8927=AXIS2_PLACEMENT_3D('',#16773,#10558,#10559);
#8928=AXIS2_PLACEMENT_3D('',#16824,#10561,#10562);
#8929=AXIS2_PLACEMENT_3D('',#16875,#10564,#10565);
#8930=AXIS2_PLACEMENT_3D('',#16923,#10567,#10568);
#8931=AXIS2_PLACEMENT_3D('',#16974,#10570,#10571);
#8932=AXIS2_PLACEMENT_3D('',#17025,#10573,#10574);
#8933=AXIS2_PLACEMENT_3D('',#17073,#10576,#10577);
#8934=AXIS2_PLACEMENT_3D('',#17121,#10579,#10580);
#8935=AXIS2_PLACEMENT_3D('',#17172,#10582,#10583);
#8936=AXIS2_PLACEMENT_3D('',#17223,#10585,#10586);
#8937=AXIS2_PLACEMENT_3D('',#17271,#10588,#10589);
#8938=AXIS2_PLACEMENT_3D('',#17322,#10591,#10592);
#8939=AXIS2_PLACEMENT_3D('',#17373,#10594,#10595);
#8940=AXIS2_PLACEMENT_3D('',#17421,#10597,#10598);
#8941=AXIS2_PLACEMENT_3D('',#17469,#10600,#10601);
#8942=AXIS2_PLACEMENT_3D('',#17520,#10603,#10604);
#8943=AXIS2_PLACEMENT_3D('',#17571,#10606,#10607);
#8944=AXIS2_PLACEMENT_3D('',#17619,#10609,#10610);
#8945=AXIS2_PLACEMENT_3D('',#17670,#10612,#10613);
#8946=AXIS2_PLACEMENT_3D('',#17721,#10615,#10616);
#8947=AXIS2_PLACEMENT_3D('',#17769,#10618,#10619);
#8948=AXIS2_PLACEMENT_3D('',#17817,#10621,#10622);
#8949=AXIS2_PLACEMENT_3D('',#17868,#10624,#10625);
#8950=AXIS2_PLACEMENT_3D('',#17934,#10627,#10628);
#8951=AXIS2_PLACEMENT_3D('',#18024,#10630,#10631);
#8952=AXIS2_PLACEMENT_3D('',#18111,#10633,#10634);
#8953=AXIS2_PLACEMENT_3D('',#18198,#10636,#10637);
#8954=AXIS2_PLACEMENT_3D('',#18285,#10639,#10640);
#8955=AXIS2_PLACEMENT_3D('',#18372,#10642,#10643);
#8956=AXIS2_PLACEMENT_3D('',#18459,#10645,#10646);
#8957=AXIS2_PLACEMENT_3D('',#18549,#10648,#10649);
#8958=AXIS2_PLACEMENT_3D('',#18558,#10651,#10652);
#8959=AXIS2_PLACEMENT_3D('',#18559,#10653,#10654);
#8960=AXIS2_PLACEMENT_3D('',#18581,#10656,#10657);
#8961=AXIS2_PLACEMENT_3D('',#18595,#10658,#10659);
#8962=AXIS2_PLACEMENT_3D('',#18633,#10661,#10662);
#8963=AXIS2_PLACEMENT_3D('',#18669,#10664,#10665);
#8964=AXIS2_PLACEMENT_3D('',#18707,#10667,#10668);
#8965=AXIS2_PLACEMENT_3D('',#18743,#10670,#10671);
#8966=AXIS2_PLACEMENT_3D('',#18781,#10673,#10674);
#8967=AXIS2_PLACEMENT_3D('',#18818,#10676,#10677);
#8968=AXIS2_PLACEMENT_3D('',#18853,#10679,#10680);
#8969=AXIS2_PLACEMENT_3D('',#18880,#10682,#10683);
#8970=AXIS2_PLACEMENT_3D('',#18904,#10685,#10686);
#8971=AXIS2_PLACEMENT_3D('',#18928,#10688,#10689);
#8972=AXIS2_PLACEMENT_3D('',#18952,#10691,#10692);
#8973=AXIS2_PLACEMENT_3D('',#18978,#10694,#10695);
#8974=AXIS2_PLACEMENT_3D('',#19002,#10697,#10698);
#8975=AXIS2_PLACEMENT_3D('',#19026,#10700,#10701);
#8976=AXIS2_PLACEMENT_3D('',#19052,#10703,#10704);
#8977=AXIS2_PLACEMENT_3D('',#19076,#10706,#10707);
#8978=AXIS2_PLACEMENT_3D('',#19100,#10709,#10710);
#8979=AXIS2_PLACEMENT_3D('',#19124,#10712,#10713);
#8980=AXIS2_PLACEMENT_3D('',#19150,#10715,#10716);
#8981=AXIS2_PLACEMENT_3D('',#19174,#10718,#10719);
#8982=AXIS2_PLACEMENT_3D('',#19198,#10721,#10722);
#8983=AXIS2_PLACEMENT_3D('',#19224,#10724,#10725);
#8984=AXIS2_PLACEMENT_3D('',#19248,#10727,#10728);
#8985=AXIS2_PLACEMENT_3D('',#19272,#10730,#10731);
#8986=AXIS2_PLACEMENT_3D('',#19296,#10733,#10734);
#8987=AXIS2_PLACEMENT_3D('',#19322,#10736,#10737);
#8988=AXIS2_PLACEMENT_3D('',#19346,#10739,#10740);
#8989=AXIS2_PLACEMENT_3D('',#19370,#10742,#10743);
#8990=AXIS2_PLACEMENT_3D('',#19396,#10745,#10746);
#8991=AXIS2_PLACEMENT_3D('',#19420,#10748,#10749);
#8992=AXIS2_PLACEMENT_3D('',#19444,#10751,#10752);
#8993=AXIS2_PLACEMENT_3D('',#19468,#10754,#10755);
#8994=AXIS2_PLACEMENT_3D('',#19494,#10757,#10758);
#8995=AXIS2_PLACEMENT_3D('',#19518,#10760,#10761);
#8996=AXIS2_PLACEMENT_3D('',#19542,#10763,#10764);
#8997=AXIS2_PLACEMENT_3D('',#19568,#10766,#10767);
#8998=AXIS2_PLACEMENT_3D('',#19592,#10769,#10770);
#8999=AXIS2_PLACEMENT_3D('',#19616,#10772,#10773);
#9000=AXIS2_PLACEMENT_3D('',#19640,#10775,#10776);
#9001=AXIS2_PLACEMENT_3D('',#19666,#10778,#10779);
#9002=AXIS2_PLACEMENT_3D('',#19690,#10781,#10782);
#9003=AXIS2_PLACEMENT_3D('',#19714,#10784,#10785);
#9004=AXIS2_PLACEMENT_3D('',#19740,#10787,#10788);
#9005=AXIS2_PLACEMENT_3D('',#19764,#10790,#10791);
#9006=AXIS2_PLACEMENT_3D('',#19788,#10793,#10794);
#9007=AXIS2_PLACEMENT_3D('',#19812,#10796,#10797);
#9008=AXIS2_PLACEMENT_3D('',#19838,#10799,#10800);
#9009=AXIS2_PLACEMENT_3D('',#19862,#10802,#10803);
#9010=AXIS2_PLACEMENT_3D('',#19886,#10805,#10806);
#9011=AXIS2_PLACEMENT_3D('',#19912,#10808,#10809);
#9012=AXIS2_PLACEMENT_3D('',#19936,#10811,#10812);
#9013=AXIS2_PLACEMENT_3D('',#19960,#10814,#10815);
#9014=AXIS2_PLACEMENT_3D('',#19985,#10817,#10818);
#9015=AXIS2_PLACEMENT_3D('',#20012,#10820,#10821);
#9016=AXIS2_PLACEMENT_3D('',#20049,#10823,#10824);
#9017=AXIS2_PLACEMENT_3D('',#20085,#10826,#10827);
#9018=AXIS2_PLACEMENT_3D('',#20123,#10829,#10830);
#9019=AXIS2_PLACEMENT_3D('',#20159,#10832,#10833);
#9020=AXIS2_PLACEMENT_3D('',#20197,#10835,#10836);
#9021=AXIS2_PLACEMENT_3D('',#20234,#10838,#10839);
#9022=AXIS2_PLACEMENT_3D('',#22382,#10841,#10842);
#9023=AXIS2_PLACEMENT_3D('',#22384,#10843,#10844);
#9024=AXIS2_PLACEMENT_3D('',#24476,#10845,#10846);
#9025=AXIS2_PLACEMENT_3D('',#24485,#10851,#10852);
#9026=AXIS2_PLACEMENT_3D('',#24487,#10853,#10854);
#9027=AXIS2_PLACEMENT_3D('',#24491,#10857,#10858);
#9028=AXIS2_PLACEMENT_3D('',#24495,#10861,#10862);
#9029=AXIS2_PLACEMENT_3D('',#24499,#10865,#10866);
#9030=AXIS2_PLACEMENT_3D('',#24500,#10867,#10868);
#9031=AXIS2_PLACEMENT_3D('',#24501,#10869,#10870);
#9032=AXIS2_PLACEMENT_3D('',#24503,#10871,#10872);
#9033=AXIS2_PLACEMENT_3D('',#24506,#10874,#10875);
#9034=AXIS2_PLACEMENT_3D('',#24507,#10876,#10877);
#9035=AXIS2_PLACEMENT_3D('',#24508,#10878,#10879);
#9036=AXIS2_PLACEMENT_3D('',#24510,#10880,#10881);
#9037=AXIS2_PLACEMENT_3D('',#24511,#10882,#10883);
#9038=AXIS2_PLACEMENT_3D('',#24512,#10884,#10885);
#9039=AXIS2_PLACEMENT_3D('',#24514,#10886,#10887);
#9040=AXIS2_PLACEMENT_3D('',#24516,#10889,#10890);
#9041=AXIS2_PLACEMENT_3D('',#24517,#10891,#10892);
#9042=AXIS2_PLACEMENT_3D('',#24518,#10893,#10894);
#9043=AXIS2_PLACEMENT_3D('',#24519,#10895,#10896);
#9044=AXIS2_PLACEMENT_3D('',#24520,#10897,#10898);
#9045=AXIS2_PLACEMENT_3D('',#24522,#10899,#10900);
#9046=AXIS2_PLACEMENT_3D('',#24525,#10902,#10903);
#9047=AXIS2_PLACEMENT_3D('',#24526,#10904,#10905);
#9048=AXIS2_PLACEMENT_3D('',#24528,#10906,#10907);
#9049=AXIS2_PLACEMENT_3D('',#24531,#10909,#10910);
#9050=AXIS2_PLACEMENT_3D('',#24532,#10911,#10912);
#9051=AXIS2_PLACEMENT_3D('',#24533,#10913,#10914);
#9052=AXIS2_PLACEMENT_3D('',#24534,#10915,#10916);
#9053=AXIS2_PLACEMENT_3D('',#24535,#10917,#10918);
#9054=AXIS2_PLACEMENT_3D('',#24539,#10920,#10921);
#9055=AXIS2_PLACEMENT_3D('',#24540,#10922,#10923);
#9056=AXIS2_PLACEMENT_3D('',#24552,#10924,#10925);
#9057=AXIS2_PLACEMENT_3D('',#24614,#10927,#10928);
#9058=AXIS2_PLACEMENT_3D('',#24616,#10930,#10931);
#9059=AXIS2_PLACEMENT_3D('',#24618,#10932,#10933);
#9060=AXIS2_PLACEMENT_3D('',#24621,#10935,#10936);
#9061=AXIS2_PLACEMENT_3D('',#24622,#10937,#10938);
#9062=AXIS2_PLACEMENT_3D('',#24624,#10939,#10940);
#9063=AXIS2_PLACEMENT_3D('',#24627,#10942,#10943);
#9064=AXIS2_PLACEMENT_3D('',#24628,#10944,#10945);
#9065=AXIS2_PLACEMENT_3D('',#24629,#10946,#10947);
#9066=AXIS2_PLACEMENT_3D('',#24630,#10948,#10949);
#9067=AXIS2_PLACEMENT_3D('',#24631,#10950,#10951);
#9068=AXIS2_PLACEMENT_3D('',#24633,#10952,#10953);
#9069=AXIS2_PLACEMENT_3D('',#24636,#10955,#10956);
#9070=AXIS2_PLACEMENT_3D('',#24637,#10957,#10958);
#9071=AXIS2_PLACEMENT_3D('',#24641,#10960,#10961);
#9072=AXIS2_PLACEMENT_3D('',#24642,#10962,#10963);
#9073=AXIS2_PLACEMENT_3D('',#24652,#10964,#10965);
#9074=AXIS2_PLACEMENT_3D('',#24708,#10967,#10968);
#9075=AXIS2_PLACEMENT_3D('',#24710,#10970,#10971);
#9076=AXIS2_PLACEMENT_3D('',#24723,#10978,#10979);
#9077=AXIS2_PLACEMENT_3D('',#24729,#10983,#10984);
#9078=AXIS2_PLACEMENT_3D('',#24739,#10990,#10991);
#9079=AXIS2_PLACEMENT_3D('',#24741,#10992,#10993);
#9080=AXIS2_PLACEMENT_3D('',#24742,#10994,#10995);
#9081=AXIS2_PLACEMENT_3D('',#24743,#10996,#10997);
#9082=AXIS2_PLACEMENT_3D('',#24745,#10998,#10999);
#9083=AXIS2_PLACEMENT_3D('',#24746,#11000,#11001);
#9084=AXIS2_PLACEMENT_3D('',#24747,#11002,#11003);
#9085=AXIS2_PLACEMENT_3D('',#24749,#11005,#11006);
#9086=AXIS2_PLACEMENT_3D('',#24750,#11007,#11008);
#9087=AXIS2_PLACEMENT_3D('',#24751,#11009,#11010);
#9088=AXIS2_PLACEMENT_3D('',#24752,#11011,#11012);
#9089=AXIS2_PLACEMENT_3D('',#24753,#11013,#11014);
#9090=AXIS2_PLACEMENT_3D('',#24754,#11015,#11016);
#9091=AXIS2_PLACEMENT_3D('',#24755,#11017,#11018);
#9092=AXIS2_PLACEMENT_3D('',#24757,#11019,#11020);
#9093=AXIS2_PLACEMENT_3D('',#24760,#11022,#11023);
#9094=AXIS2_PLACEMENT_3D('',#24761,#11024,#11025);
#9095=AXIS2_PLACEMENT_3D('',#24763,#11026,#11027);
#9096=AXIS2_PLACEMENT_3D('',#24766,#11029,#11030);
#9097=AXIS2_PLACEMENT_3D('',#24767,#11031,#11032);
#9098=AXIS2_PLACEMENT_3D('',#24768,#11033,#11034);
#9099=AXIS2_PLACEMENT_3D('',#24769,#11035,#11036);
#9100=AXIS2_PLACEMENT_3D('',#24770,#11037,#11038);
#9101=AXIS2_PLACEMENT_3D('',#24772,#11039,#11040);
#9102=AXIS2_PLACEMENT_3D('',#24775,#11042,#11043);
#9103=AXIS2_PLACEMENT_3D('',#24776,#11044,#11045);
#9104=AXIS2_PLACEMENT_3D('',#24778,#11046,#11047);
#9105=AXIS2_PLACEMENT_3D('',#24781,#11049,#11050);
#9106=AXIS2_PLACEMENT_3D('',#24782,#11051,#11052);
#9107=AXIS2_PLACEMENT_3D('',#24783,#11053,#11054);
#9108=AXIS2_PLACEMENT_3D('',#24784,#11055,#11056);
#9109=AXIS2_PLACEMENT_3D('',#24785,#11057,#11058);
#9110=AXIS2_PLACEMENT_3D('',#24802,#11067,#11068);
#9111=AXIS2_PLACEMENT_3D('',#24808,#11072,#11073);
#9112=AXIS2_PLACEMENT_3D('',#24812,#11076,#11077);
#9113=AXIS2_PLACEMENT_3D('',#24816,#11080,#11081);
#9114=AXIS2_PLACEMENT_3D('',#24820,#11084,#11085);
#9115=AXIS2_PLACEMENT_3D('',#24828,#11090,#11091);
#9116=AXIS2_PLACEMENT_3D('',#24830,#11093,#11094);
#9117=AXIS2_PLACEMENT_3D('',#24832,#11096,#11097);
#9118=AXIS2_PLACEMENT_3D('',#24834,#11099,#11100);
#9119=AXIS2_PLACEMENT_3D('',#24835,#11101,#11102);
#9120=AXIS2_PLACEMENT_3D('',#24836,#11103,#11104);
#9121=AXIS2_PLACEMENT_3D('',#24845,#11109,#11110);
#9122=AXIS2_PLACEMENT_3D('',#24851,#11114,#11115);
#9123=AXIS2_PLACEMENT_3D('',#24857,#11119,#11120);
#9124=AXIS2_PLACEMENT_3D('',#24863,#11124,#11125);
#9125=AXIS2_PLACEMENT_3D('',#24869,#11129,#11130);
#9126=AXIS2_PLACEMENT_3D('',#24872,#11133,#11134);
#9127=AXIS2_PLACEMENT_3D('',#24873,#11135,#11136);
#9128=AXIS2_PLACEMENT_3D('',#24875,#11137,#11138);
#9129=AXIS2_PLACEMENT_3D('',#24876,#11139,#11140);
#9130=AXIS2_PLACEMENT_3D('',#24878,#11141,#11142);
#9131=AXIS2_PLACEMENT_3D('',#24880,#11144,#11145);
#9132=AXIS2_PLACEMENT_3D('',#24882,#11146,#11147);
#9133=AXIS2_PLACEMENT_3D('',#24884,#11149,#11150);
#9134=AXIS2_PLACEMENT_3D('',#24886,#11151,#11152);
#9135=AXIS2_PLACEMENT_3D('',#24888,#11154,#11155);
#9136=AXIS2_PLACEMENT_3D('',#24889,#11156,#11157);
#9137=AXIS2_PLACEMENT_3D('',#24890,#11158,#11159);
#9138=AXIS2_PLACEMENT_3D('',#24892,#11160,#11161);
#9139=AXIS2_PLACEMENT_3D('',#24895,#11163,#11164);
#9140=AXIS2_PLACEMENT_3D('',#24896,#11165,#11166);
#9141=AXIS2_PLACEMENT_3D('',#24898,#11167,#11168);
#9142=AXIS2_PLACEMENT_3D('',#24901,#11170,#11171);
#9143=AXIS2_PLACEMENT_3D('',#24902,#11172,#11173);
#9144=AXIS2_PLACEMENT_3D('',#24903,#11174,#11175);
#9145=AXIS2_PLACEMENT_3D('',#24904,#11176,#11177);
#9146=AXIS2_PLACEMENT_3D('',#24905,#11178,#11179);
#9147=AXIS2_PLACEMENT_3D('',#24907,#11180,#11181);
#9148=AXIS2_PLACEMENT_3D('',#24908,#11182,#11183);
#9149=AXIS2_PLACEMENT_3D('',#24910,#11184,#11185);
#9150=AXIS2_PLACEMENT_3D('',#24912,#11187,#11188);
#9151=AXIS2_PLACEMENT_3D('',#24914,#11189,#11190);
#9152=AXIS2_PLACEMENT_3D('',#24916,#11192,#11193);
#9153=AXIS2_PLACEMENT_3D('',#24918,#11194,#11195);
#9154=AXIS2_PLACEMENT_3D('',#24920,#11197,#11198);
#9155=AXIS2_PLACEMENT_3D('',#24922,#11199,#11200);
#9156=AXIS2_PLACEMENT_3D('',#24923,#11201,#11202);
#9157=AXIS2_PLACEMENT_3D('',#24925,#11203,#11204);
#9158=AXIS2_PLACEMENT_3D('',#24927,#11206,#11207);
#9159=AXIS2_PLACEMENT_3D('',#24929,#11208,#11209);
#9160=AXIS2_PLACEMENT_3D('',#24931,#11211,#11212);
#9161=AXIS2_PLACEMENT_3D('',#24933,#11213,#11214);
#9162=AXIS2_PLACEMENT_3D('',#24935,#11216,#11217);
#9163=AXIS2_PLACEMENT_3D('',#24936,#11218,#11219);
#9164=AXIS2_PLACEMENT_3D('',#24945,#11224,#11225);
#9165=AXIS2_PLACEMENT_3D('',#24951,#11229,#11230);
#9166=AXIS2_PLACEMENT_3D('',#24957,#11234,#11235);
#9167=AXIS2_PLACEMENT_3D('',#24963,#11239,#11240);
#9168=AXIS2_PLACEMENT_3D('',#24969,#11244,#11245);
#9169=AXIS2_PLACEMENT_3D('',#24972,#11248,#11249);
#9170=AXIS2_PLACEMENT_3D('',#24973,#11250,#11251);
#9171=AXIS2_PLACEMENT_3D('',#24974,#11252,#11253);
#9172=AXIS2_PLACEMENT_3D('',#24975,#11254,#11255);
#9173=AXIS2_PLACEMENT_3D('',#24976,#11256,#11257);
#9174=AXIS2_PLACEMENT_3D('',#24977,#11258,#11259);
#9175=AXIS2_PLACEMENT_3D('',#24978,#11260,#11261);
#9176=AXIS2_PLACEMENT_3D('',#24979,#11262,#11263);
#9177=AXIS2_PLACEMENT_3D('',#24980,#11264,#11265);
#9178=AXIS2_PLACEMENT_3D('',#24981,#11266,#11267);
#9179=AXIS2_PLACEMENT_3D('',#24982,#11268,#11269);
#9180=AXIS2_PLACEMENT_3D('',#24983,#11270,#11271);
#9181=AXIS2_PLACEMENT_3D('',#24984,#11272,#11273);
#9182=AXIS2_PLACEMENT_3D('',#24985,#11274,#11275);
#9183=AXIS2_PLACEMENT_3D('',#24986,#11276,#11277);
#9184=AXIS2_PLACEMENT_3D('',#24987,#11278,#11279);
#9185=AXIS2_PLACEMENT_3D('',#24988,#11280,#11281);
#9186=AXIS2_PLACEMENT_3D('',#24989,#11282,#11283);
#9187=AXIS2_PLACEMENT_3D('',#24990,#11284,#11285);
#9188=AXIS2_PLACEMENT_3D('',#24991,#11286,#11287);
#9189=AXIS2_PLACEMENT_3D('',#24992,#11288,#11289);
#9190=AXIS2_PLACEMENT_3D('',#24993,#11290,#11291);
#9191=AXIS2_PLACEMENT_3D('',#24994,#11292,#11293);
#9192=AXIS2_PLACEMENT_3D('',#24995,#11294,#11295);
#9193=AXIS2_PLACEMENT_3D('',#24996,#11296,#11297);
#9194=AXIS2_PLACEMENT_3D('',#24997,#11298,#11299);
#9195=AXIS2_PLACEMENT_3D('',#24998,#11300,#11301);
#9196=AXIS2_PLACEMENT_3D('',#24999,#11302,#11303);
#9197=AXIS2_PLACEMENT_3D('',#25000,#11304,#11305);
#9198=AXIS2_PLACEMENT_3D('',#25001,#11306,#11307);
#9199=AXIS2_PLACEMENT_3D('',#25002,#11308,#11309);
#9200=AXIS2_PLACEMENT_3D('',#25003,#11310,#11311);
#9201=AXIS2_PLACEMENT_3D('',#25004,#11312,#11313);
#9202=AXIS2_PLACEMENT_3D('',#25005,#11314,#11315);
#9203=AXIS2_PLACEMENT_3D('',#25006,#11316,#11317);
#9204=DIRECTION('axis',(0.,0.,1.));
#9205=DIRECTION('refdir',(1.,0.,0.));
#9206=DIRECTION('axis',(0.,0.,1.));
#9207=DIRECTION('refdir',(1.,0.,0.));
#9208=DIRECTION('axis',(0.,0.,1.));
#9209=DIRECTION('refdir',(1.,0.,0.));
#9210=DIRECTION('center_axis',(0.,0.,1.));
#9211=DIRECTION('ref_axis',(1.,0.,0.));
#9212=DIRECTION('center_axis',(0.,0.,1.));
#9213=DIRECTION('ref_axis',(1.,0.,0.));
#9214=DIRECTION('',(0.,0.,1.));
#9215=DIRECTION('center_axis',(0.,0.,-1.));
#9216=DIRECTION('ref_axis',(1.,0.,0.));
#9217=DIRECTION('center_axis',(0.,0.,1.));
#9218=DIRECTION('ref_axis',(1.,0.,0.));
#9219=DIRECTION('center_axis',(0.,0.,1.));
#9220=DIRECTION('ref_axis',(1.,0.,0.));
#9221=DIRECTION('',(0.,0.,1.));
#9222=DIRECTION('center_axis',(0.,0.,-1.));
#9223=DIRECTION('ref_axis',(1.,0.,0.));
#9224=DIRECTION('center_axis',(0.,0.,1.));
#9225=DIRECTION('ref_axis',(1.,0.,0.));
#9226=DIRECTION('center_axis',(0.,0.,1.));
#9227=DIRECTION('ref_axis',(1.,0.,0.));
#9228=DIRECTION('',(0.,0.,1.));
#9229=DIRECTION('center_axis',(0.,0.,-1.));
#9230=DIRECTION('ref_axis',(1.,0.,0.));
#9231=DIRECTION('center_axis',(0.,0.,1.));
#9232=DIRECTION('ref_axis',(1.,0.,0.));
#9233=DIRECTION('center_axis',(0.,0.,1.));
#9234=DIRECTION('ref_axis',(1.,0.,0.));
#9235=DIRECTION('',(0.,0.,1.));
#9236=DIRECTION('center_axis',(0.,0.,-1.));
#9237=DIRECTION('ref_axis',(1.,0.,0.));
#9238=DIRECTION('center_axis',(0.,0.,1.));
#9239=DIRECTION('ref_axis',(1.,0.,0.));
#9240=DIRECTION('center_axis',(0.,0.,1.));
#9241=DIRECTION('ref_axis',(1.,0.,0.));
#9242=DIRECTION('',(0.,0.,1.));
#9243=DIRECTION('center_axis',(0.,0.,-1.));
#9244=DIRECTION('ref_axis',(1.,0.,0.));
#9245=DIRECTION('center_axis',(0.,0.,1.));
#9246=DIRECTION('ref_axis',(1.,0.,0.));
#9247=DIRECTION('center_axis',(0.,0.,1.));
#9248=DIRECTION('ref_axis',(1.,0.,0.));
#9249=DIRECTION('',(0.,0.,1.));
#9250=DIRECTION('center_axis',(0.,0.,-1.));
#9251=DIRECTION('ref_axis',(1.,0.,0.));
#9252=DIRECTION('center_axis',(0.,0.,1.));
#9253=DIRECTION('ref_axis',(1.,0.,0.));
#9254=DIRECTION('center_axis',(0.,0.,1.));
#9255=DIRECTION('ref_axis',(1.,0.,0.));
#9256=DIRECTION('',(0.,0.,1.));
#9257=DIRECTION('center_axis',(0.,0.,-1.));
#9258=DIRECTION('ref_axis',(1.,0.,0.));
#9259=DIRECTION('center_axis',(0.,1.,0.));
#9260=DIRECTION('ref_axis',(-1.,0.,0.));
#9261=DIRECTION('',(-1.,0.,0.));
#9262=DIRECTION('',(0.,0.,1.));
#9263=DIRECTION('',(-1.,0.,0.));
#9264=DIRECTION('',(0.,0.,1.));
#9265=DIRECTION('center_axis',(1.,0.,0.));
#9266=DIRECTION('ref_axis',(0.,1.,0.));
#9267=DIRECTION('',(0.,1.,0.));
#9268=DIRECTION('',(0.,1.,0.));
#9269=DIRECTION('',(0.,0.,1.));
#9270=DIRECTION('center_axis',(0.,-1.,0.));
#9271=DIRECTION('ref_axis',(1.,0.,0.));
#9272=DIRECTION('',(1.,0.,0.));
#9273=DIRECTION('',(1.,0.,0.));
#9274=DIRECTION('',(0.,0.,1.));
#9275=DIRECTION('center_axis',(-1.,0.,0.));
#9276=DIRECTION('ref_axis',(0.,-1.,0.));
#9277=DIRECTION('',(0.,-1.,0.));
#9278=DIRECTION('',(0.,-1.,0.));
#9279=DIRECTION('center_axis',(0.,0.,1.));
#9280=DIRECTION('ref_axis',(1.,0.,0.));
#9281=DIRECTION('center_axis',(0.,0.,1.));
#9282=DIRECTION('ref_axis',(1.,0.,0.));
#9283=DIRECTION('axis',(0.,0.,1.));
#9284=DIRECTION('refdir',(1.,0.,0.));
#9285=DIRECTION('center_axis',(0.,0.,1.));
#9286=DIRECTION('ref_axis',(1.,0.,0.));
#9287=DIRECTION('center_axis',(0.,0.,1.));
#9288=DIRECTION('ref_axis',(1.,0.,0.));
#9289=DIRECTION('',(0.,0.,1.));
#9290=DIRECTION('center_axis',(0.,0.,1.));
#9291=DIRECTION('ref_axis',(1.,0.,0.));
#9292=DIRECTION('center_axis',(0.,0.,1.));
#9293=DIRECTION('ref_axis',(1.,0.,0.));
#9294=DIRECTION('center_axis',(0.,0.,1.));
#9295=DIRECTION('ref_axis',(1.,0.,0.));
#9296=DIRECTION('center_axis',(0.,0.,1.));
#9297=DIRECTION('ref_axis',(1.,0.,0.));
#9298=DIRECTION('',(0.,0.,1.));
#9299=DIRECTION('center_axis',(0.,0.,1.));
#9300=DIRECTION('ref_axis',(1.,0.,0.));
#9301=DIRECTION('center_axis',(0.,0.,1.));
#9302=DIRECTION('ref_axis',(1.,0.,0.));
#9303=DIRECTION('center_axis',(0.,0.,1.));
#9304=DIRECTION('ref_axis',(1.,0.,0.));
#9305=DIRECTION('center_axis',(0.,0.,1.));
#9306=DIRECTION('ref_axis',(1.,0.,0.));
#9307=DIRECTION('',(0.,0.,1.));
#9308=DIRECTION('center_axis',(0.,0.,1.));
#9309=DIRECTION('ref_axis',(1.,0.,0.));
#9310=DIRECTION('center_axis',(0.,0.,1.));
#9311=DIRECTION('ref_axis',(1.,0.,0.));
#9312=DIRECTION('center_axis',(0.,0.,1.));
#9313=DIRECTION('ref_axis',(0.,-1.,0.));
#9314=DIRECTION('',(0.,-1.,0.));
#9315=DIRECTION('',(1.,0.,0.));
#9316=DIRECTION('',(0.,-1.,0.));
#9317=DIRECTION('',(1.,0.,0.));
#9318=DIRECTION('center_axis',(0.,0.894427190999916,-0.447213595499958));
#9319=DIRECTION('ref_axis',(0.,0.447213595499958,0.894427190999916));
#9320=DIRECTION('',(0.,0.447213595499958,0.894427190999916));
#9321=DIRECTION('',(0.,0.447213595499958,0.894427190999916));
#9322=DIRECTION('',(1.,0.,0.));
#9323=DIRECTION('center_axis',(0.,0.,-1.));
#9324=DIRECTION('ref_axis',(0.,1.,0.));
#9325=DIRECTION('',(0.,1.,0.));
#9326=DIRECTION('',(0.,1.,0.));
#9327=DIRECTION('',(1.,0.,0.));
#9328=DIRECTION('center_axis',(0.,-0.894427190999916,-0.447213595499958));
#9329=DIRECTION('ref_axis',(0.,0.447213595499958,-0.894427190999916));
#9330=DIRECTION('',(0.,0.447213595499958,-0.894427190999916));
#9331=DIRECTION('',(0.,0.447213595499958,-0.894427190999916));
#9332=DIRECTION('center_axis',(1.,0.,0.));
#9333=DIRECTION('ref_axis',(0.,0.,-1.));
#9334=DIRECTION('center_axis',(1.,0.,0.));
#9335=DIRECTION('ref_axis',(0.,0.,-1.));
#9336=DIRECTION('axis',(0.,0.,1.));
#9337=DIRECTION('refdir',(1.,0.,0.));
#9338=DIRECTION('center_axis',(1.,0.,0.));
#9339=DIRECTION('ref_axis',(0.,0.,-1.));
#9340=DIRECTION('center_axis',(1.,0.,0.));
#9341=DIRECTION('ref_axis',(0.,0.,-1.));
#9342=DIRECTION('',(1.,0.,0.));
#9343=DIRECTION('center_axis',(-1.,0.,0.));
#9344=DIRECTION('ref_axis',(0.,0.,-1.));
#9345=DIRECTION('center_axis',(1.,0.,0.));
#9346=DIRECTION('ref_axis',(0.,0.,-1.));
#9347=DIRECTION('center_axis',(1.,0.,0.));
#9348=DIRECTION('ref_axis',(0.,0.,-1.));
#9349=DIRECTION('center_axis',(1.,0.,0.));
#9350=DIRECTION('ref_axis',(0.,0.,-1.));
#9351=DIRECTION('',(1.,0.,0.));
#9352=DIRECTION('center_axis',(-1.,0.,0.));
#9353=DIRECTION('ref_axis',(0.,0.,-1.));
#9354=DIRECTION('center_axis',(1.,0.,0.));
#9355=DIRECTION('ref_axis',(0.,0.,-1.));
#9356=DIRECTION('center_axis',(0.,0.,1.));
#9357=DIRECTION('ref_axis',(1.,0.,0.));
#9358=DIRECTION('center_axis',(0.,0.,1.));
#9359=DIRECTION('ref_axis',(1.,0.,0.));
#9360=DIRECTION('',(0.,0.,1.));
#9361=DIRECTION('center_axis',(0.,0.,1.));
#9362=DIRECTION('ref_axis',(1.,0.,0.));
#9363=DIRECTION('center_axis',(0.,0.,1.));
#9364=DIRECTION('ref_axis',(1.,0.,0.));
#9365=DIRECTION('center_axis',(0.,0.,1.));
#9366=DIRECTION('ref_axis',(1.,0.,0.));
#9367=DIRECTION('center_axis',(0.,0.,1.));
#9368=DIRECTION('ref_axis',(1.,0.,0.));
#9369=DIRECTION('',(0.,0.,1.));
#9370=DIRECTION('center_axis',(0.,0.,1.));
#9371=DIRECTION('ref_axis',(1.,0.,0.));
#9372=DIRECTION('center_axis',(0.,0.,1.));
#9373=DIRECTION('ref_axis',(1.,0.,0.));
#9374=DIRECTION('center_axis',(0.,1.,0.));
#9375=DIRECTION('ref_axis',(-1.,0.,0.));
#9376=DIRECTION('',(-1.,0.,0.));
#9377=DIRECTION('',(0.,0.,1.));
#9378=DIRECTION('',(-1.,0.,0.));
#9379=DIRECTION('',(0.,0.,1.));
#9380=DIRECTION('center_axis',(1.,0.,0.));
#9381=DIRECTION('ref_axis',(0.,1.,0.));
#9382=DIRECTION('',(0.,1.,0.));
#9383=DIRECTION('',(0.,1.,0.));
#9384=DIRECTION('',(0.,0.,1.));
#9385=DIRECTION('center_axis',(0.,-1.,0.));
#9386=DIRECTION('ref_axis',(1.,0.,0.));
#9387=DIRECTION('',(1.,0.,0.));
#9388=DIRECTION('',(1.,0.,0.));
#9389=DIRECTION('',(0.,0.,1.));
#9390=DIRECTION('center_axis',(-1.,0.,0.));
#9391=DIRECTION('ref_axis',(0.,-1.,0.));
#9392=DIRECTION('',(0.,-1.,0.));
#9393=DIRECTION('',(0.,-1.,0.));
#9394=DIRECTION('center_axis',(0.,0.,1.));
#9395=DIRECTION('ref_axis',(1.,0.,0.));
#9396=DIRECTION('center_axis',(0.,0.,1.));
#9397=DIRECTION('ref_axis',(1.,0.,0.));
#9398=DIRECTION('axis',(0.,0.,1.));
#9399=DIRECTION('refdir',(1.,0.,0.));
#9400=DIRECTION('center_axis',(1.,0.,0.));
#9401=DIRECTION('ref_axis',(0.,0.,-1.));
#9402=DIRECTION('center_axis',(1.,0.,0.));
#9403=DIRECTION('ref_axis',(0.,0.,-1.));
#9404=DIRECTION('',(1.,0.,0.));
#9405=DIRECTION('center_axis',(-1.,0.,0.));
#9406=DIRECTION('ref_axis',(0.,0.,-1.));
#9407=DIRECTION('center_axis',(1.,0.,0.));
#9408=DIRECTION('ref_axis',(0.,0.,-1.));
#9409=DIRECTION('center_axis',(1.,0.,0.));
#9410=DIRECTION('ref_axis',(0.,0.,-1.));
#9411=DIRECTION('',(1.,0.,0.));
#9412=DIRECTION('center_axis',(-1.,0.,0.));
#9413=DIRECTION('ref_axis',(0.,0.,-1.));
#9414=DIRECTION('center_axis',(1.,0.,0.));
#9415=DIRECTION('ref_axis',(0.,0.,-1.));
#9416=DIRECTION('center_axis',(1.,0.,0.));
#9417=DIRECTION('ref_axis',(0.,0.,-1.));
#9418=DIRECTION('',(1.,0.,0.));
#9419=DIRECTION('center_axis',(-1.,0.,0.));
#9420=DIRECTION('ref_axis',(0.,0.,-1.));
#9421=DIRECTION('center_axis',(1.,0.,0.));
#9422=DIRECTION('ref_axis',(0.,0.,-1.));
#9423=DIRECTION('center_axis',(1.,0.,0.));
#9424=DIRECTION('ref_axis',(0.,0.,-1.));
#9425=DIRECTION('',(1.,0.,0.));
#9426=DIRECTION('center_axis',(-1.,0.,0.));
#9427=DIRECTION('ref_axis',(0.,0.,-1.));
#9428=DIRECTION('center_axis',(1.,0.,0.));
#9429=DIRECTION('ref_axis',(0.,0.,-1.));
#9430=DIRECTION('center_axis',(1.,0.,0.));
#9431=DIRECTION('ref_axis',(0.,0.,-1.));
#9432=DIRECTION('center_axis',(1.,0.,0.));
#9433=DIRECTION('ref_axis',(0.,0.,-1.));
#9434=DIRECTION('center_axis',(1.,0.,0.));
#9435=DIRECTION('ref_axis',(0.,0.,-1.));
#9436=DIRECTION('',(1.,0.,0.));
#9437=DIRECTION('center_axis',(0.,0.,1.));
#9438=DIRECTION('ref_axis',(1.,0.,0.));
#9439=DIRECTION('center_axis',(0.,0.,1.));
#9440=DIRECTION('ref_axis',(1.,0.,0.));
#9441=DIRECTION('',(0.,0.,1.));
#9442=DIRECTION('center_axis',(0.,0.,1.));
#9443=DIRECTION('ref_axis',(1.,0.,0.));
#9444=DIRECTION('center_axis',(0.,0.,1.));
#9445=DIRECTION('ref_axis',(1.,0.,0.));
#9446=DIRECTION('center_axis',(0.,0.,1.));
#9447=DIRECTION('ref_axis',(1.,0.,0.));
#9448=DIRECTION('center_axis',(0.,0.,1.));
#9449=DIRECTION('ref_axis',(1.,0.,0.));
#9450=DIRECTION('',(0.,0.,1.));
#9451=DIRECTION('center_axis',(0.,0.,1.));
#9452=DIRECTION('ref_axis',(1.,0.,0.));
#9453=DIRECTION('center_axis',(0.,0.,1.));
#9454=DIRECTION('ref_axis',(1.,0.,0.));
#9455=DIRECTION('center_axis',(0.,1.,0.));
#9456=DIRECTION('ref_axis',(-1.,0.,0.));
#9457=DIRECTION('',(-1.,0.,0.));
#9458=DIRECTION('',(0.,0.,1.));
#9459=DIRECTION('',(-1.,0.,0.));
#9460=DIRECTION('',(0.,0.,1.));
#9461=DIRECTION('center_axis',(1.,0.,0.));
#9462=DIRECTION('ref_axis',(0.,1.,0.));
#9463=DIRECTION('',(0.,1.,0.));
#9464=DIRECTION('',(0.,1.,0.));
#9465=DIRECTION('',(0.,0.,1.));
#9466=DIRECTION('center_axis',(0.,-1.,0.));
#9467=DIRECTION('ref_axis',(1.,0.,0.));
#9468=DIRECTION('',(1.,0.,0.));
#9469=DIRECTION('',(1.,0.,0.));
#9470=DIRECTION('',(0.,0.,1.));
#9471=DIRECTION('center_axis',(-1.,0.,0.));
#9472=DIRECTION('ref_axis',(0.,-1.,0.));
#9473=DIRECTION('',(0.,-1.,0.));
#9474=DIRECTION('',(0.,-1.,0.));
#9475=DIRECTION('center_axis',(0.,0.,1.));
#9476=DIRECTION('ref_axis',(1.,0.,0.));
#9477=DIRECTION('center_axis',(0.,0.,1.));
#9478=DIRECTION('ref_axis',(1.,0.,0.));
#9479=DIRECTION('axis',(0.,0.,1.));
#9480=DIRECTION('refdir',(1.,0.,0.));
#9481=DIRECTION('center_axis',(1.,0.,0.));
#9482=DIRECTION('ref_axis',(0.,0.,-1.));
#9483=DIRECTION('center_axis',(1.,0.,0.));
#9484=DIRECTION('ref_axis',(0.,0.,-1.));
#9485=DIRECTION('',(1.,0.,0.));
#9486=DIRECTION('center_axis',(-1.,0.,0.));
#9487=DIRECTION('ref_axis',(0.,0.,-1.));
#9488=DIRECTION('center_axis',(1.,0.,0.));
#9489=DIRECTION('ref_axis',(0.,0.,-1.));
#9490=DIRECTION('center_axis',(1.,0.,0.));
#9491=DIRECTION('ref_axis',(0.,0.,-1.));
#9492=DIRECTION('',(1.,0.,0.));
#9493=DIRECTION('center_axis',(-1.,0.,0.));
#9494=DIRECTION('ref_axis',(0.,0.,-1.));
#9495=DIRECTION('center_axis',(1.,0.,0.));
#9496=DIRECTION('ref_axis',(0.,0.,-1.));
#9497=DIRECTION('center_axis',(1.,0.,0.));
#9498=DIRECTION('ref_axis',(0.,0.,-1.));
#9499=DIRECTION('',(1.,0.,0.));
#9500=DIRECTION('center_axis',(-1.,0.,0.));
#9501=DIRECTION('ref_axis',(0.,0.,-1.));
#9502=DIRECTION('center_axis',(0.,0.,1.));
#9503=DIRECTION('ref_axis',(0.,-1.,0.));
#9504=DIRECTION('',(1.,0.,0.));
#9505=DIRECTION('',(0.,-1.,0.));
#9506=DIRECTION('',(-1.,0.,0.));
#9507=DIRECTION('',(0.,1.,0.));
#9508=DIRECTION('center_axis',(1.,0.,0.));
#9509=DIRECTION('ref_axis',(0.,0.,-1.));
#9510=DIRECTION('center_axis',(1.,0.,0.));
#9511=DIRECTION('ref_axis',(0.,0.,-1.));
#9512=DIRECTION('center_axis',(1.,0.,0.));
#9513=DIRECTION('ref_axis',(0.,0.,-1.));
#9514=DIRECTION('center_axis',(1.,0.,0.));
#9515=DIRECTION('ref_axis',(0.,1.22464679914735E-16,1.));
#9516=DIRECTION('center_axis',(1.,0.,0.));
#9517=DIRECTION('ref_axis',(0.,0.,-1.));
#9518=DIRECTION('center_axis',(1.,0.,0.));
#9519=DIRECTION('ref_axis',(0.,0.,-1.));
#9520=DIRECTION('',(-1.,0.,0.));
#9521=DIRECTION('center_axis',(1.,0.,0.));
#9522=DIRECTION('ref_axis',(0.,0.,-1.));
#9523=DIRECTION('center_axis',(1.,0.,0.));
#9524=DIRECTION('ref_axis',(0.,0.,-1.));
#9525=DIRECTION('center_axis',(-1.,0.,0.));
#9526=DIRECTION('ref_axis',(0.,0.,-1.));
#9527=DIRECTION('center_axis',(1.,0.,0.));
#9528=DIRECTION('ref_axis',(0.,0.,-1.));
#9529=DIRECTION('center_axis',(-1.,0.,0.));
#9530=DIRECTION('ref_axis',(0.,0.,-1.));
#9531=DIRECTION('',(-1.,0.,0.));
#9532=DIRECTION('center_axis',(1.,0.,0.));
#9533=DIRECTION('ref_axis',(0.,0.,-1.));
#9534=DIRECTION('axis',(0.,0.,1.));
#9535=DIRECTION('refdir',(1.,0.,0.));
#9536=DIRECTION('center_axis',(0.,1.,0.));
#9537=DIRECTION('ref_axis',(1.,0.,0.));
#9538=DIRECTION('',(0.,0.,1.));
#9539=DIRECTION('',(1.,0.,0.));
#9540=DIRECTION('',(0.,0.,-1.));
#9541=DIRECTION('',(-1.,0.,0.));
#9542=DIRECTION('center_axis',(-1.,0.,0.));
#9543=DIRECTION('ref_axis',(0.,-1.,0.));
#9544=DIRECTION('',(0.,-1.,0.));
#9545=DIRECTION('',(0.,0.,1.));
#9546=DIRECTION('',(0.,-1.,0.));
#9547=DIRECTION('center_axis',(1.,0.,0.));
#9548=DIRECTION('ref_axis',(0.,0.,-1.));
#9549=DIRECTION('center_axis',(1.,0.,0.));
#9550=DIRECTION('ref_axis',(0.,0.,-1.));
#9551=DIRECTION('center_axis',(0.,0.,1.));
#9552=DIRECTION('ref_axis',(1.,0.,0.));
#9553=DIRECTION('',(0.,1.,0.));
#9554=DIRECTION('',(-1.,0.,0.));
#9555=DIRECTION('center_axis',(0.,1.,0.));
#9556=DIRECTION('ref_axis',(0.,0.,1.));
#9557=DIRECTION('',(0.,0.,-1.));
#9558=DIRECTION('',(1.,0.,0.));
#9559=DIRECTION('center_axis',(1.,0.,0.));
#9560=DIRECTION('ref_axis',(0.,1.,0.));
#9561=DIRECTION('',(0.,1.,0.));
#9562=DIRECTION('center_axis',(-1.,0.,0.));
#9563=DIRECTION('ref_axis',(0.,0.,-1.));
#9564=DIRECTION('center_axis',(-1.,0.,0.));
#9565=DIRECTION('ref_axis',(0.,0.,-1.));
#9566=DIRECTION('center_axis',(1.,0.,0.));
#9567=DIRECTION('ref_axis',(0.,0.,-1.));
#9568=DIRECTION('center_axis',(1.,0.,0.));
#9569=DIRECTION('ref_axis',(0.,0.,-1.));
#9570=DIRECTION('',(1.,0.,0.));
#9571=DIRECTION('center_axis',(1.,0.,0.));
#9572=DIRECTION('ref_axis',(0.,0.,-1.));
#9573=DIRECTION('center_axis',(1.,0.,0.));
#9574=DIRECTION('ref_axis',(0.,0.,-1.));
#9575=DIRECTION('center_axis',(1.,0.,0.));
#9576=DIRECTION('ref_axis',(0.,0.,-1.));
#9577=DIRECTION('center_axis',(1.,0.,0.));
#9578=DIRECTION('ref_axis',(0.,0.,-1.));
#9579=DIRECTION('',(1.,0.,0.));
#9580=DIRECTION('center_axis',(1.,0.,0.));
#9581=DIRECTION('ref_axis',(0.,0.,-1.));
#9582=DIRECTION('center_axis',(1.,0.,0.));
#9583=DIRECTION('ref_axis',(0.,0.,-1.));
#9584=DIRECTION('center_axis',(1.,0.,0.));
#9585=DIRECTION('ref_axis',(0.,0.,-1.));
#9586=DIRECTION('',(1.,0.,0.));
#9587=DIRECTION('center_axis',(1.,0.,0.));
#9588=DIRECTION('ref_axis',(0.,0.,-1.));
#9589=DIRECTION('',(1.,0.,0.));
#9590=DIRECTION('center_axis',(0.,0.,1.));
#9591=DIRECTION('ref_axis',(1.,0.,0.));
#9592=DIRECTION('axis',(0.,0.,1.));
#9593=DIRECTION('refdir',(1.,0.,0.));
#9594=DIRECTION('center_axis',(0.866025403784439,0.,-0.5));
#9595=DIRECTION('ref_axis',(0.5,0.,0.866025403784439));
#9596=DIRECTION('',(-0.5,0.,-0.866025403784439));
#9597=DIRECTION('',(0.,-1.,0.));
#9598=DIRECTION('',(0.5,0.,0.866025403784439));
#9599=DIRECTION('',(0.,-1.,0.));
#9600=DIRECTION('center_axis',(1.92296268638356E-16,0.,-1.));
#9601=DIRECTION('ref_axis',(1.,0.,1.92296268638356E-16));
#9602=DIRECTION('',(-1.,0.,-1.92296268638356E-16));
#9603=DIRECTION('',(0.,-1.,0.));
#9604=DIRECTION('',(1.,0.,1.92296268638356E-16));
#9605=DIRECTION('center_axis',(-0.866025403784439,0.,-0.5));
#9606=DIRECTION('ref_axis',(0.5,0.,-0.866025403784439));
#9607=DIRECTION('',(-0.5,0.,0.866025403784438));
#9608=DIRECTION('',(0.,-1.,0.));
#9609=DIRECTION('',(0.5,0.,-0.866025403784438));
#9610=DIRECTION('center_axis',(-0.866025403784439,0.,0.5));
#9611=DIRECTION('ref_axis',(-0.5,0.,-0.866025403784439));
#9612=DIRECTION('',(0.5,0.,0.866025403784439));
#9613=DIRECTION('',(0.,-1.,0.));
#9614=DIRECTION('',(-0.5,0.,-0.866025403784439));
#9615=DIRECTION('center_axis',(-1.92296268638356E-16,0.,1.));
#9616=DIRECTION('ref_axis',(-1.,0.,-1.92296268638356E-16));
#9617=DIRECTION('',(1.,0.,1.92296268638356E-16));
#9618=DIRECTION('',(0.,-1.,0.));
#9619=DIRECTION('',(-1.,0.,-1.92296268638356E-16));
#9620=DIRECTION('center_axis',(0.866025403784439,0.,0.5));
#9621=DIRECTION('ref_axis',(-0.5,0.,0.866025403784439));
#9622=DIRECTION('',(0.5,0.,-0.866025403784439));
#9623=DIRECTION('',(-0.5,0.,0.866025403784439));
#9624=DIRECTION('center_axis',(0.,1.,0.));
#9625=DIRECTION('ref_axis',(1.,0.,0.));
#9626=DIRECTION('center_axis',(0.,-1.,0.));
#9627=DIRECTION('ref_axis',(0.,0.,-1.));
#9628=DIRECTION('center_axis',(0.,1.,0.));
#9629=DIRECTION('ref_axis',(1.,0.,0.));
#9630=DIRECTION('center_axis',(0.,1.,0.));
#9631=DIRECTION('ref_axis',(1.,0.,0.));
#9632=DIRECTION('center_axis',(0.,1.,0.));
#9633=DIRECTION('ref_axis',(0.,0.,1.));
#9634=DIRECTION('center_axis',(0.,-1.,0.));
#9635=DIRECTION('ref_axis',(1.,0.,0.));
#9636=DIRECTION('center_axis',(0.,-1.,0.));
#9637=DIRECTION('ref_axis',(1.,0.,0.));
#9638=DIRECTION('center_axis',(0.,-1.,0.));
#9639=DIRECTION('ref_axis',(1.,0.,0.));
#9640=DIRECTION('',(0.707106781186548,0.707106781186547,8.65956056235494E-17));
#9641=DIRECTION('center_axis',(0.,-1.,0.));
#9642=DIRECTION('ref_axis',(1.,0.,0.));
#9643=DIRECTION('center_axis',(0.,-1.,0.));
#9644=DIRECTION('ref_axis',(1.,0.,0.));
#9645=DIRECTION('',(0.,1.,0.));
#9646=DIRECTION('center_axis',(0.,1.,0.));
#9647=DIRECTION('ref_axis',(1.,0.,0.));
#9648=DIRECTION('center_axis',(0.,-1.,0.));
#9649=DIRECTION('ref_axis',(1.,0.,0.));
#9650=DIRECTION('',(-0.707106781186547,0.707106781186548,-8.65956056235493E-17));
#9651=DIRECTION('center_axis',(0.,-1.,0.));
#9652=DIRECTION('ref_axis',(0.,0.,-1.));
#9653=DIRECTION('center_axis',(0.,-1.,0.));
#9654=DIRECTION('ref_axis',(1.,0.,0.));
#9655=DIRECTION('center_axis',(0.,1.,0.));
#9656=DIRECTION('ref_axis',(1.,0.,0.));
#9657=DIRECTION('center_axis',(0.,1.,0.));
#9658=DIRECTION('ref_axis',(1.,0.,0.));
#9659=DIRECTION('',(-0.447213595499958,0.894427190999916,-5.47678698264203E-17));
#9660=DIRECTION('center_axis',(0.,-1.,0.));
#9661=DIRECTION('ref_axis',(1.,0.,0.));
#9662=DIRECTION('',(0.,1.,0.));
#9663=DIRECTION('axis',(0.,0.,1.));
#9664=DIRECTION('refdir',(1.,0.,0.));
#9665=DIRECTION('axis',(0.,0.,1.));
#9666=DIRECTION('refdir',(1.,0.,0.));
#9667=DIRECTION('center_axis',(0.,-1.,0.));
#9668=DIRECTION('ref_axis',(0.,0.,-1.));
#9669=DIRECTION('center_axis',(0.,-1.,0.));
#9670=DIRECTION('ref_axis',(1.,0.,0.));
#9671=DIRECTION('center_axis',(0.,-1.,0.));
#9672=DIRECTION('ref_axis',(1.,0.,0.));
#9673=DIRECTION('center_axis',(1.,0.,1.22464679914735E-16));
#9674=DIRECTION('ref_axis',(-1.22464679914735E-16,0.,1.));
#9675=DIRECTION('center_axis',(0.,1.,0.));
#9676=DIRECTION('ref_axis',(1.,0.,0.));
#9677=DIRECTION('center_axis',(0.,1.,0.));
#9678=DIRECTION('ref_axis',(1.,0.,0.));
#9679=DIRECTION('center_axis',(0.,-1.,0.));
#9680=DIRECTION('ref_axis',(1.,0.,0.));
#9681=DIRECTION('',(0.,1.,0.));
#9682=DIRECTION('center_axis',(0.,-1.,0.));
#9683=DIRECTION('ref_axis',(1.,0.,0.));
#9684=DIRECTION('center_axis',(0.,-1.,0.));
#9685=DIRECTION('ref_axis',(1.,0.,0.));
#9686=DIRECTION('center_axis',(0.,-1.,0.));
#9687=DIRECTION('ref_axis',(1.,0.,0.));
#9688=DIRECTION('',(0.,1.,0.));
#9689=DIRECTION('center_axis',(0.,-1.,0.));
#9690=DIRECTION('ref_axis',(1.,0.,0.));
#9691=DIRECTION('center_axis',(0.,1.,0.));
#9692=DIRECTION('ref_axis',(1.,0.,0.));
#9693=DIRECTION('',(-0.707106781186548,0.707106781186547,-8.65956056235494E-17));
#9694=DIRECTION('center_axis',(0.,-1.,0.));
#9695=DIRECTION('ref_axis',(1.,0.,0.));
#9696=DIRECTION('center_axis',(0.,1.,0.));
#9697=DIRECTION('ref_axis',(0.,0.,1.));
#9698=DIRECTION('center_axis',(0.,-1.,0.));
#9699=DIRECTION('ref_axis',(1.,0.,0.));
#9700=DIRECTION('center_axis',(0.,-1.,0.));
#9701=DIRECTION('ref_axis',(1.,0.,0.));
#9702=DIRECTION('',(0.,1.,0.));
#9703=DIRECTION('center_axis',(0.,-1.,0.));
#9704=DIRECTION('ref_axis',(0.,0.,-1.));
#9705=DIRECTION('center_axis',(0.,-1.,0.));
#9706=DIRECTION('ref_axis',(1.,0.,0.));
#9707=DIRECTION('center_axis',(0.,-1.,0.));
#9708=DIRECTION('ref_axis',(1.,0.,0.));
#9709=DIRECTION('',(0.707106781186548,0.707106781186547,8.65956056235494E-17));
#9710=DIRECTION('axis',(0.,0.,1.));
#9711=DIRECTION('refdir',(1.,0.,0.));
#9712=DIRECTION('center_axis',(0.,-1.,0.));
#9713=DIRECTION('ref_axis',(0.,0.,-1.));
#9714=DIRECTION('center_axis',(0.,-1.,0.));
#9715=DIRECTION('ref_axis',(1.,0.,0.));
#9716=DIRECTION('center_axis',(0.,-1.,0.));
#9717=DIRECTION('ref_axis',(1.,0.,0.));
#9718=DIRECTION('center_axis',(1.,0.,1.22464679914735E-16));
#9719=DIRECTION('ref_axis',(-1.22464679914735E-16,0.,1.));
#9720=DIRECTION('center_axis',(0.,1.,0.));
#9721=DIRECTION('ref_axis',(1.,0.,0.));
#9722=DIRECTION('center_axis',(0.,1.,0.));
#9723=DIRECTION('ref_axis',(1.,0.,0.));
#9724=DIRECTION('center_axis',(0.,-1.,0.));
#9725=DIRECTION('ref_axis',(1.,0.,0.));
#9726=DIRECTION('center_axis',(0.,-1.,0.));
#9727=DIRECTION('ref_axis',(1.,0.,0.));
#9728=DIRECTION('',(0.,1.,0.));
#9729=DIRECTION('center_axis',(0.,1.,0.));
#9730=DIRECTION('ref_axis',(0.,0.,1.));
#9731=DIRECTION('center_axis',(0.,-1.,0.));
#9732=DIRECTION('ref_axis',(1.,0.,0.));
#9733=DIRECTION('center_axis',(0.,-1.,0.));
#9734=DIRECTION('ref_axis',(1.,0.,0.));
#9735=DIRECTION('center_axis',(0.,-1.,0.));
#9736=DIRECTION('ref_axis',(1.,0.,0.));
#9737=DIRECTION('center_axis',(0.,-1.,0.));
#9738=DIRECTION('ref_axis',(1.,0.,0.));
#9739=DIRECTION('',(0.707106781186548,0.707106781186547,8.65956056235494E-17));
#9740=DIRECTION('center_axis',(0.,-1.,0.));
#9741=DIRECTION('ref_axis',(1.,0.,0.));
#9742=DIRECTION('center_axis',(0.,-1.,0.));
#9743=DIRECTION('ref_axis',(1.,0.,0.));
#9744=DIRECTION('',(0.,1.,0.));
#9745=DIRECTION('center_axis',(0.,1.,0.));
#9746=DIRECTION('ref_axis',(1.,0.,0.));
#9747=DIRECTION('center_axis',(0.,-1.,0.));
#9748=DIRECTION('ref_axis',(1.,0.,0.));
#9749=DIRECTION('',(-0.707106781186548,0.707106781186547,-8.65956056235494E-17));
#9750=DIRECTION('center_axis',(0.,-1.,0.));
#9751=DIRECTION('ref_axis',(0.,0.,-1.));
#9752=DIRECTION('center_axis',(0.,-1.,0.));
#9753=DIRECTION('ref_axis',(1.,0.,0.));
#9754=DIRECTION('',(0.,1.,0.));
#9755=DIRECTION('axis',(0.,0.,1.));
#9756=DIRECTION('refdir',(1.,0.,0.));
#9757=DIRECTION('center_axis',(0.,0.,1.));
#9758=DIRECTION('ref_axis',(1.,0.,0.));
#9759=DIRECTION('center_axis',(1.22464679914735E-16,-1.,0.));
#9760=DIRECTION('ref_axis',(-1.,-1.22464679914735E-16,0.));
#9761=DIRECTION('center_axis',(0.707106781186548,0.,0.707106781186548));
#9762=DIRECTION('ref_axis',(0.707106781186548,0.,-0.707106781186548));
#9763=DIRECTION('center_axis',(8.65956056235493E-17,-1.,-8.65956056235493E-17));
#9764=DIRECTION('ref_axis',(-0.707106781186548,-1.22464679914735E-16,0.707106781186548));
#9765=DIRECTION('center_axis',(1.,0.,0.));
#9766=DIRECTION('ref_axis',(6.12323399573677E-17,0.,-1.));
#9767=DIRECTION('center_axis',(7.49879891330929E-33,-1.,-1.22464679914735E-16));
#9768=DIRECTION('ref_axis',(-6.12323399573677E-17,-1.22464679914735E-16,
1.));
#9769=DIRECTION('center_axis',(0.707106781186548,0.,-0.707106781186548));
#9770=DIRECTION('ref_axis',(-0.707106781186548,0.,-0.707106781186548));
#9771=DIRECTION('center_axis',(-8.65956056235493E-17,-1.,-8.65956056235493E-17));
#9772=DIRECTION('ref_axis',(0.707106781186548,-1.22464679914735E-16,0.707106781186548));
#9773=DIRECTION('center_axis',(0.,0.,-1.));
#9774=DIRECTION('ref_axis',(-1.,0.,-1.22464679914735E-16));
#9775=DIRECTION('center_axis',(-1.22464679914735E-16,-1.,-1.49975978266186E-32));
#9776=DIRECTION('ref_axis',(1.,-1.22464679914735E-16,1.22464679914735E-16));
#9777=DIRECTION('center_axis',(-0.707106781186548,0.,-0.707106781186548));
#9778=DIRECTION('ref_axis',(-0.707106781186548,0.,0.707106781186548));
#9779=DIRECTION('center_axis',(-8.65956056235493E-17,-1.,8.65956056235493E-17));
#9780=DIRECTION('ref_axis',(0.707106781186548,-1.22464679914735E-16,-0.707106781186548));
#9781=DIRECTION('center_axis',(-1.,0.,0.));
#9782=DIRECTION('ref_axis',(-1.83697019872103E-16,0.,1.));
#9783=DIRECTION('center_axis',(-2.24963967399279E-32,-1.,1.22464679914735E-16));
#9784=DIRECTION('ref_axis',(1.83697019872103E-16,-1.22464679914735E-16,
-1.));
#9785=DIRECTION('center_axis',(-0.707106781186548,0.,0.707106781186548));
#9786=DIRECTION('ref_axis',(0.707106781186548,0.,0.707106781186548));
#9787=DIRECTION('center_axis',(8.65956056235493E-17,-1.,8.65956056235494E-17));
#9788=DIRECTION('ref_axis',(-0.707106781186548,-1.22464679914735E-16,-0.707106781186548));
#9789=DIRECTION('axis',(0.,0.,1.));
#9790=DIRECTION('refdir',(1.,0.,0.));
#9791=DIRECTION('center_axis',(0.,0.,1.));
#9792=DIRECTION('ref_axis',(1.,0.,0.));
#9793=DIRECTION('center_axis',(0.,-1.,0.));
#9794=DIRECTION('ref_axis',(0.,0.,-1.));
#9795=DIRECTION('center_axis',(0.,-1.,0.));
#9796=DIRECTION('ref_axis',(0.,0.,-1.));
#9797=DIRECTION('center_axis',(0.,1.,0.));
#9798=DIRECTION('ref_axis',(1.,0.,0.));
#9799=DIRECTION('center_axis',(0.,1.,0.));
#9800=DIRECTION('ref_axis',(1.,0.,0.));
#9801=DIRECTION('center_axis',(0.,1.,0.));
#9802=DIRECTION('ref_axis',(1.,0.,0.));
#9803=DIRECTION('center_axis',(0.,1.,0.));
#9804=DIRECTION('ref_axis',(1.,0.,0.));
#9805=DIRECTION('',(0.,-1.,0.));
#9806=DIRECTION('center_axis',(0.,-1.,0.));
#9807=DIRECTION('ref_axis',(1.,0.,0.));
#9808=DIRECTION('center_axis',(0.,1.,0.));
#9809=DIRECTION('ref_axis',(1.,0.,0.));
#9810=DIRECTION('center_axis',(0.,1.,0.));
#9811=DIRECTION('ref_axis',(1.,0.,0.));
#9812=DIRECTION('center_axis',(0.,1.,0.));
#9813=DIRECTION('ref_axis',(1.,0.,0.));
#9814=DIRECTION('center_axis',(0.,1.,0.));
#9815=DIRECTION('ref_axis',(1.,0.,0.));
#9816=DIRECTION('center_axis',(0.,1.,0.));
#9817=DIRECTION('ref_axis',(1.,0.,0.));
#9818=DIRECTION('center_axis',(0.,1.,0.));
#9819=DIRECTION('ref_axis',(1.,0.,0.));
#9820=DIRECTION('center_axis',(0.,-1.,0.));
#9821=DIRECTION('ref_axis',(1.,0.,0.));
#9822=DIRECTION('center_axis',(0.,-1.,0.));
#9823=DIRECTION('ref_axis',(0.,0.,-1.));
#9824=DIRECTION('center_axis',(6.12323399573677E-17,0.,1.));
#9825=DIRECTION('ref_axis',(1.,0.,0.));
#9826=DIRECTION('center_axis',(0.,-1.,0.));
#9827=DIRECTION('ref_axis',(0.,0.,-1.));
#9828=DIRECTION('center_axis',(0.,1.,0.));
#9829=DIRECTION('ref_axis',(1.,0.,0.));
#9830=DIRECTION('center_axis',(0.,-1.,0.));
#9831=DIRECTION('ref_axis',(1.,0.,0.));
#9832=DIRECTION('center_axis',(0.,-1.,0.));
#9833=DIRECTION('ref_axis',(0.,0.,-1.));
#9834=DIRECTION('center_axis',(0.,0.,1.));
#9835=DIRECTION('ref_axis',(1.,0.,0.));
#9836=DIRECTION('center_axis',(0.,-1.,0.));
#9837=DIRECTION('ref_axis',(0.,0.,-1.));
#9838=DIRECTION('center_axis',(0.,1.,0.));
#9839=DIRECTION('ref_axis',(1.,0.,0.));
#9840=DIRECTION('center_axis',(0.,-1.,0.));
#9841=DIRECTION('ref_axis',(1.,0.,0.));
#9842=DIRECTION('center_axis',(0.,-1.,0.));
#9843=DIRECTION('ref_axis',(0.,0.,-1.));
#9844=DIRECTION('center_axis',(0.,0.,1.));
#9845=DIRECTION('ref_axis',(1.,0.,0.));
#9846=DIRECTION('center_axis',(0.,-1.,0.));
#9847=DIRECTION('ref_axis',(0.,0.,-1.));
#9848=DIRECTION('center_axis',(0.,1.,0.));
#9849=DIRECTION('ref_axis',(1.,0.,0.));
#9850=DIRECTION('center_axis',(0.,-1.,0.));
#9851=DIRECTION('ref_axis',(1.,0.,0.));
#9852=DIRECTION('center_axis',(0.,-1.,0.));
#9853=DIRECTION('ref_axis',(0.,0.,-1.));
#9854=DIRECTION('center_axis',(0.,0.,1.));
#9855=DIRECTION('ref_axis',(1.,0.,0.));
#9856=DIRECTION('center_axis',(0.,-1.,0.));
#9857=DIRECTION('ref_axis',(0.,0.,-1.));
#9858=DIRECTION('center_axis',(0.,1.,0.));
#9859=DIRECTION('ref_axis',(1.,0.,0.));
#9860=DIRECTION('center_axis',(0.,-1.,0.));
#9861=DIRECTION('ref_axis',(1.,0.,0.));
#9862=DIRECTION('center_axis',(0.,-1.,0.));
#9863=DIRECTION('ref_axis',(0.,0.,-1.));
#9864=DIRECTION('center_axis',(6.12323399573676E-17,0.,1.));
#9865=DIRECTION('ref_axis',(1.,0.,0.));
#9866=DIRECTION('center_axis',(0.,-1.,0.));
#9867=DIRECTION('ref_axis',(0.,0.,-1.));
#9868=DIRECTION('center_axis',(0.,1.,0.));
#9869=DIRECTION('ref_axis',(1.,0.,0.));
#9870=DIRECTION('center_axis',(0.,-1.,0.));
#9871=DIRECTION('ref_axis',(1.,0.,0.));
#9872=DIRECTION('center_axis',(0.,-1.,0.));
#9873=DIRECTION('ref_axis',(0.,0.,-1.));
#9874=DIRECTION('center_axis',(0.,0.,1.));
#9875=DIRECTION('ref_axis',(1.,0.,0.));
#9876=DIRECTION('center_axis',(0.,-1.,0.));
#9877=DIRECTION('ref_axis',(0.,0.,-1.));
#9878=DIRECTION('center_axis',(0.,1.,0.));
#9879=DIRECTION('ref_axis',(1.,0.,0.));
#9880=DIRECTION('center_axis',(0.,1.,0.));
#9881=DIRECTION('ref_axis',(1.,0.,0.));
#9882=DIRECTION('',(0.,1.,0.));
#9883=DIRECTION('center_axis',(0.,-1.,0.));
#9884=DIRECTION('ref_axis',(1.,0.,0.));
#9885=DIRECTION('center_axis',(0.,-1.,0.));
#9886=DIRECTION('ref_axis',(1.,0.,0.));
#9887=DIRECTION('center_axis',(0.,1.,0.));
#9888=DIRECTION('ref_axis',(1.,0.,0.));
#9889=DIRECTION('center_axis',(0.,-1.,0.));
#9890=DIRECTION('ref_axis',(0.,0.,-1.));
#9891=DIRECTION('center_axis',(0.,0.,1.));
#9892=DIRECTION('ref_axis',(1.,0.,0.));
#9893=DIRECTION('center_axis',(0.,-1.,0.));
#9894=DIRECTION('ref_axis',(0.,0.,-1.));
#9895=DIRECTION('center_axis',(0.,-1.,0.));
#9896=DIRECTION('ref_axis',(-1.,0.,0.));
#9897=DIRECTION('center_axis',(0.,1.,0.));
#9898=DIRECTION('ref_axis',(1.,0.,0.));
#9899=DIRECTION('axis',(0.,0.,1.));
#9900=DIRECTION('refdir',(1.,0.,0.));
#9901=DIRECTION('center_axis',(0.,1.,0.));
#9902=DIRECTION('ref_axis',(0.,0.,1.));
#9903=DIRECTION('center_axis',(0.,-1.,0.));
#9904=DIRECTION('ref_axis',(1.,0.,0.));
#9905=DIRECTION('center_axis',(0.,-1.,0.));
#9906=DIRECTION('ref_axis',(1.,0.,0.));
#9907=DIRECTION('center_axis',(0.,-1.,0.));
#9908=DIRECTION('ref_axis',(1.,0.,0.));
#9909=DIRECTION('center_axis',(0.,-1.,0.));
#9910=DIRECTION('ref_axis',(1.,0.,0.));
#9911=DIRECTION('',(0.,1.,0.));
#9912=DIRECTION('center_axis',(0.,-1.,0.));
#9913=DIRECTION('ref_axis',(0.,0.,-1.));
#9914=DIRECTION('center_axis',(0.,-1.,0.));
#9915=DIRECTION('ref_axis',(1.,0.,0.));
#9916=DIRECTION('center_axis',(0.,-1.,0.));
#9917=DIRECTION('ref_axis',(1.,0.,0.));
#9918=DIRECTION('',(0.,1.,0.));
#9919=DIRECTION('center_axis',(0.,1.,0.));
#9920=DIRECTION('ref_axis',(0.,0.,1.));
#9921=DIRECTION('center_axis',(0.,-1.,0.));
#9922=DIRECTION('ref_axis',(1.,0.,0.));
#9923=DIRECTION('center_axis',(0.,-1.,0.));
#9924=DIRECTION('ref_axis',(1.,0.,0.));
#9925=DIRECTION('center_axis',(0.,-1.,0.));
#9926=DIRECTION('ref_axis',(1.,0.,0.));
#9927=DIRECTION('center_axis',(0.,-1.,0.));
#9928=DIRECTION('ref_axis',(1.,0.,0.));
#9929=DIRECTION('',(0.,1.,0.));
#9930=DIRECTION('center_axis',(0.,-1.,0.));
#9931=DIRECTION('ref_axis',(0.,0.,-1.));
#9932=DIRECTION('center_axis',(0.,-1.,0.));
#9933=DIRECTION('ref_axis',(1.,0.,0.));
#9934=DIRECTION('center_axis',(0.,-1.,0.));
#9935=DIRECTION('ref_axis',(1.,0.,0.));
#9936=DIRECTION('',(0.,1.,0.));
#9937=DIRECTION('',(0.,0.,1.));
#9938=DIRECTION('',(1.,0.,0.));
#9939=DIRECTION('',(0.,0.,1.));
#9940=DIRECTION('',(1.,0.,0.));
#9941=DIRECTION('',(0.,0.,1.));
#9942=DIRECTION('',(1.,0.,0.));
#9943=DIRECTION('',(0.,0.,1.));
#9944=DIRECTION('',(1.,0.,0.));
#9945=DIRECTION('',(0.,0.,1.));
#9946=DIRECTION('',(1.,0.,0.));
#9947=DIRECTION('axis',(0.,0.,1.));
#9948=DIRECTION('refdir',(1.,0.,0.));
#9949=DIRECTION('axis',(0.,0.,1.));
#9950=DIRECTION('refdir',(1.,0.,0.));
#9951=DIRECTION('center_axis',(1.,0.,0.));
#9952=DIRECTION('ref_axis',(0.,0.,-1.));
#9953=DIRECTION('center_axis',(1.,0.,0.));
#9954=DIRECTION('ref_axis',(0.,0.,-1.));
#9955=DIRECTION('',(1.,0.,0.));
#9956=DIRECTION('center_axis',(-1.,0.,0.));
#9957=DIRECTION('ref_axis',(0.,0.,-1.));
#9958=DIRECTION('center_axis',(1.,0.,0.));
#9959=DIRECTION('ref_axis',(0.,0.,-1.));
#9960=DIRECTION('center_axis',(1.,0.,0.));
#9961=DIRECTION('ref_axis',(0.,0.,-1.));
#9962=DIRECTION('center_axis',(1.,0.,0.));
#9963=DIRECTION('ref_axis',(0.,0.,-1.));
#9964=DIRECTION('',(1.,0.,0.));
#9965=DIRECTION('center_axis',(-1.,0.,0.));
#9966=DIRECTION('ref_axis',(0.,0.,-1.));
#9967=DIRECTION('center_axis',(1.,0.,0.));
#9968=DIRECTION('ref_axis',(0.,0.,-1.));
#9969=DIRECTION('center_axis',(1.,0.,0.));
#9970=DIRECTION('ref_axis',(0.,0.,-1.));
#9971=DIRECTION('center_axis',(1.,0.,0.));
#9972=DIRECTION('ref_axis',(0.,0.,-1.));
#9973=DIRECTION('',(1.,0.,0.));
#9974=DIRECTION('center_axis',(-1.,0.,0.));
#9975=DIRECTION('ref_axis',(0.,0.,-1.));
#9976=DIRECTION('center_axis',(1.,0.,0.));
#9977=DIRECTION('ref_axis',(0.,0.,-1.));
#9978=DIRECTION('center_axis',(1.,0.,0.));
#9979=DIRECTION('ref_axis',(0.,0.,-1.));
#9980=DIRECTION('center_axis',(1.,0.,0.));
#9981=DIRECTION('ref_axis',(0.,0.,-1.));
#9982=DIRECTION('',(1.,0.,0.));
#9983=DIRECTION('center_axis',(1.,0.,0.));
#9984=DIRECTION('ref_axis',(0.,0.,-1.));
#9985=DIRECTION('center_axis',(1.,0.,0.));
#9986=DIRECTION('ref_axis',(0.,0.,-1.));
#9987=DIRECTION('center_axis',(1.,0.,0.));
#9988=DIRECTION('ref_axis',(0.,0.,-1.));
#9989=DIRECTION('center_axis',(1.,0.,0.));
#9990=DIRECTION('ref_axis',(0.,0.,-1.));
#9991=DIRECTION('',(1.,0.,0.));
#9992=DIRECTION('center_axis',(1.,0.,0.));
#9993=DIRECTION('ref_axis',(0.,0.,-1.));
#9994=DIRECTION('center_axis',(1.,0.,0.));
#9995=DIRECTION('ref_axis',(0.,0.,-1.));
#9996=DIRECTION('center_axis',(0.,1.,0.));
#9997=DIRECTION('ref_axis',(1.,0.,0.));
#9998=DIRECTION('center_axis',(0.,1.,0.));
#9999=DIRECTION('ref_axis',(1.,0.,0.));
#10000=DIRECTION('',(0.,1.,0.));
#10001=DIRECTION('center_axis',(0.,-1.,0.));
#10002=DIRECTION('ref_axis',(1.,0.,0.));
#10003=DIRECTION('center_axis',(0.,1.,0.));
#10004=DIRECTION('ref_axis',(1.,0.,0.));
#10005=DIRECTION('center_axis',(0.,1.,0.));
#10006=DIRECTION('ref_axis',(1.,0.,0.));
#10007=DIRECTION('center_axis',(0.,1.,0.));
#10008=DIRECTION('ref_axis',(1.,0.,0.));
#10009=DIRECTION('center_axis',(0.,1.,0.));
#10010=DIRECTION('ref_axis',(1.,0.,0.));
#10011=DIRECTION('',(0.,1.,0.));
#10012=DIRECTION('center_axis',(0.,1.,0.));
#10013=DIRECTION('ref_axis',(1.,0.,0.));
#10014=DIRECTION('center_axis',(0.,1.,0.));
#10015=DIRECTION('ref_axis',(1.,0.,0.));
#10016=DIRECTION('',(0.,1.,0.));
#10017=DIRECTION('center_axis',(0.,-1.,0.));
#10018=DIRECTION('ref_axis',(1.,0.,0.));
#10019=DIRECTION('center_axis',(0.,1.,0.));
#10020=DIRECTION('ref_axis',(1.,0.,0.));
#10021=DIRECTION('center_axis',(0.,1.,0.));
#10022=DIRECTION('ref_axis',(1.,0.,0.));
#10023=DIRECTION('center_axis',(0.,1.,0.));
#10024=DIRECTION('ref_axis',(1.,0.,0.));
#10025=DIRECTION('center_axis',(0.,1.,0.));
#10026=DIRECTION('ref_axis',(1.,0.,0.));
#10027=DIRECTION('',(0.,1.,0.));
#10028=DIRECTION('center_axis',(1.,0.,0.));
#10029=DIRECTION('ref_axis',(0.,0.,-1.));
#10030=DIRECTION('center_axis',(1.,0.,0.));
#10031=DIRECTION('ref_axis',(0.,0.,-1.));
#10032=DIRECTION('',(1.,0.,0.));
#10033=DIRECTION('center_axis',(-1.,0.,0.));
#10034=DIRECTION('ref_axis',(0.,0.,-1.));
#10035=DIRECTION('center_axis',(0.,1.,0.));
#10036=DIRECTION('ref_axis',(0.,0.,1.));
#10037=DIRECTION('',(0.,0.,-1.));
#10038=DIRECTION('',(1.,0.,0.));
#10039=DIRECTION('',(0.,0.,1.));
#10040=DIRECTION('',(-1.,0.,0.));
#10041=DIRECTION('center_axis',(0.,0.,1.));
#10042=DIRECTION('ref_axis',(0.,-1.,0.));
#10043=DIRECTION('',(0.,1.,0.));
#10044=DIRECTION('',(1.,0.,0.));
#10045=DIRECTION('',(0.,-1.,0.));
#10046=DIRECTION('center_axis',(0.,-0.921146216293932,-0.389216711110112));
#10047=DIRECTION('ref_axis',(0.,0.389216711110112,-0.921146216293932));
#10048=DIRECTION('',(0.,-0.389216711110112,0.921146216293932));
#10049=DIRECTION('',(1.,0.,0.));
#10050=DIRECTION('',(0.,0.389216711110112,-0.921146216293932));
#10051=DIRECTION('center_axis',(1.,0.,0.));
#10052=DIRECTION('ref_axis',(0.,1.,0.));
#10053=DIRECTION('',(0.,1.,0.));
#10054=DIRECTION('',(0.,0.,1.));
#10055=DIRECTION('',(0.,1.,0.));
#10056=DIRECTION('',(0.,0.,1.));
#10057=DIRECTION('',(0.,1.,0.));
#10058=DIRECTION('center_axis',(0.,0.,1.));
#10059=DIRECTION('ref_axis',(1.,0.,0.));
#10060=DIRECTION('',(0.,-1.,0.));
#10061=DIRECTION('',(-1.,0.,0.));
#10062=DIRECTION('center_axis',(0.,1.,0.));
#10063=DIRECTION('ref_axis',(-1.,0.,0.));
#10064=DIRECTION('',(0.,0.,1.));
#10065=DIRECTION('',(-1.,0.,0.));
#10066=DIRECTION('center_axis',(0.,-1.,0.));
#10067=DIRECTION('ref_axis',(1.,0.,0.));
#10068=DIRECTION('',(1.,0.,0.));
#10069=DIRECTION('',(1.,0.,0.));
#10070=DIRECTION('',(0.,0.,1.));
#10071=DIRECTION('center_axis',(-1.,0.,0.));
#10072=DIRECTION('ref_axis',(0.,-1.,0.));
#10073=DIRECTION('',(0.,-1.,0.));
#10074=DIRECTION('',(0.,-1.,0.));
#10075=DIRECTION('center_axis',(0.,0.,1.));
#10076=DIRECTION('ref_axis',(1.,0.,0.));
#10077=DIRECTION('center_axis',(0.,0.,1.));
#10078=DIRECTION('ref_axis',(1.,0.,0.));
#10079=DIRECTION('axis',(0.,0.,1.));
#10080=DIRECTION('refdir',(1.,0.,0.));
#10081=DIRECTION('center_axis',(0.,0.,1.));
#10082=DIRECTION('ref_axis',(0.,-1.,0.));
#10083=DIRECTION('',(0.,-1.,0.));
#10084=DIRECTION('',(1.,0.,0.));
#10085=DIRECTION('',(0.,-1.,0.));
#10086=DIRECTION('',(1.,0.,0.));
#10087=DIRECTION('center_axis',(0.,1.,0.));
#10088=DIRECTION('ref_axis',(0.,0.,1.));
#10089=DIRECTION('',(0.,0.,1.));
#10090=DIRECTION('',(0.,0.,1.));
#10091=DIRECTION('',(1.,0.,0.));
#10092=DIRECTION('center_axis',(0.,0.,-1.));
#10093=DIRECTION('ref_axis',(0.,1.,0.));
#10094=DIRECTION('',(0.,1.,0.));
#10095=DIRECTION('',(0.,1.,0.));
#10096=DIRECTION('',(1.,0.,0.));
#10097=DIRECTION('center_axis',(0.,-0.894427190999916,0.447213595499958));
#10098=DIRECTION('ref_axis',(0.,-0.447213595499958,-0.894427190999916));
#10099=DIRECTION('',(0.,-0.447213595499958,-0.894427190999916));
#10100=DIRECTION('',(0.,-0.447213595499958,-0.894427190999916));
#10101=DIRECTION('center_axis',(1.,0.,0.));
#10102=DIRECTION('ref_axis',(0.,0.,-1.));
#10103=DIRECTION('center_axis',(1.,0.,0.));
#10104=DIRECTION('ref_axis',(0.,0.,-1.));
#10105=DIRECTION('axis',(0.,0.,1.));
#10106=DIRECTION('refdir',(1.,0.,0.));
#10107=DIRECTION('center_axis',(0.,1.,0.));
#10108=DIRECTION('ref_axis',(1.,0.,0.));
#10109=DIRECTION('',(0.,0.,1.));
#10110=DIRECTION('',(1.,0.,0.));
#10111=DIRECTION('',(0.,0.,-1.));
#10112=DIRECTION('',(-1.,0.,0.));
#10113=DIRECTION('center_axis',(-1.,0.,0.));
#10114=DIRECTION('ref_axis',(0.,-1.,0.));
#10115=DIRECTION('',(0.,-1.,0.));
#10116=DIRECTION('',(0.,0.,1.));
#10117=DIRECTION('',(0.,-1.,0.));
#10118=DIRECTION('center_axis',(1.,0.,0.));
#10119=DIRECTION('ref_axis',(0.,0.,-1.));
#10120=DIRECTION('center_axis',(1.,0.,0.));
#10121=DIRECTION('ref_axis',(0.,0.,-1.));
#10122=DIRECTION('center_axis',(0.,0.,1.));
#10123=DIRECTION('ref_axis',(1.,0.,0.));
#10124=DIRECTION('',(0.,1.,0.));
#10125=DIRECTION('',(-1.,0.,0.));
#10126=DIRECTION('center_axis',(0.,1.,0.));
#10127=DIRECTION('ref_axis',(0.,0.,1.));
#10128=DIRECTION('',(0.,0.,-1.));
#10129=DIRECTION('',(1.,0.,0.));
#10130=DIRECTION('center_axis',(1.,0.,0.));
#10131=DIRECTION('ref_axis',(0.,1.,0.));
#10132=DIRECTION('',(0.,1.,0.));
#10133=DIRECTION('center_axis',(-1.,0.,0.));
#10134=DIRECTION('ref_axis',(0.,0.,-1.));
#10135=DIRECTION('center_axis',(-1.,0.,0.));
#10136=DIRECTION('ref_axis',(0.,0.,-1.));
#10137=DIRECTION('center_axis',(1.,0.,0.));
#10138=DIRECTION('ref_axis',(0.,0.,-1.));
#10139=DIRECTION('',(1.,0.,0.));
#10140=DIRECTION('center_axis',(1.,0.,0.));
#10141=DIRECTION('ref_axis',(0.,0.,-1.));
#10142=DIRECTION('center_axis',(1.,0.,0.));
#10143=DIRECTION('ref_axis',(0.,0.,-1.));
#10144=DIRECTION('center_axis',(-1.,0.,0.));
#10145=DIRECTION('ref_axis',(0.,0.,-1.));
#10146=DIRECTION('center_axis',(1.,0.,0.));
#10147=DIRECTION('ref_axis',(0.,0.,-1.));
#10148=DIRECTION('',(1.,0.,0.));
#10149=DIRECTION('center_axis',(1.,0.,0.));
#10150=DIRECTION('ref_axis',(0.,0.,-1.));
#10151=DIRECTION('center_axis',(1.,0.,0.));
#10152=DIRECTION('ref_axis',(0.,0.,-1.));
#10153=DIRECTION('center_axis',(-1.,0.,0.));
#10154=DIRECTION('ref_axis',(0.,0.,-1.));
#10155=DIRECTION('center_axis',(1.,0.,0.));
#10156=DIRECTION('ref_axis',(0.,0.,-1.));
#10157=DIRECTION('',(1.,0.,0.));
#10158=DIRECTION('center_axis',(1.,0.,0.));
#10159=DIRECTION('ref_axis',(0.,0.,-1.));
#10160=DIRECTION('',(1.,0.,0.));
#10161=DIRECTION('center_axis',(0.,0.,1.));
#10162=DIRECTION('ref_axis',(1.,0.,0.));
#10163=DIRECTION('axis',(0.,0.,1.));
#10164=DIRECTION('refdir',(1.,0.,0.));
#10165=DIRECTION('center_axis',(1.,0.,0.));
#10166=DIRECTION('ref_axis',(0.,0.207879895528894,-0.978154358490978));
#10167=DIRECTION('',(-1.,0.,0.));
#10168=DIRECTION('center_axis',(1.,0.,0.));
#10169=DIRECTION('ref_axis',(0.,0.,-1.));
#10170=DIRECTION('center_axis',(1.,0.,0.));
#10171=DIRECTION('ref_axis',(0.,0.,-1.));
#10172=DIRECTION('',(-1.,0.,0.));
#10173=DIRECTION('center_axis',(1.,0.,0.));
#10174=DIRECTION('ref_axis',(0.,0.,-1.));
#10175=DIRECTION('',(-1.,0.,0.));
#10176=DIRECTION('center_axis',(1.,0.,0.));
#10177=DIRECTION('ref_axis',(0.,0.,-1.));
#10178=DIRECTION('',(-1.,0.,0.));
#10179=DIRECTION('center_axis',(1.,0.,0.));
#10180=DIRECTION('ref_axis',(0.,0.,-1.));
#10181=DIRECTION('',(-1.,0.,0.));
#10182=DIRECTION('center_axis',(1.,0.,0.));
#10183=DIRECTION('ref_axis',(0.,0.,-1.));
#10184=DIRECTION('',(-1.,0.,0.));
#10185=DIRECTION('center_axis',(1.,0.,0.));
#10186=DIRECTION('ref_axis',(0.,0.,-1.));
#10187=DIRECTION('',(-1.,0.,0.));
#10188=DIRECTION('center_axis',(1.,0.,0.));
#10189=DIRECTION('ref_axis',(0.,0.,-1.));
#10190=DIRECTION('',(-1.,0.,0.));
#10191=DIRECTION('center_axis',(1.,0.,0.));
#10192=DIRECTION('ref_axis',(0.,0.,-1.));
#10193=DIRECTION('',(-1.,0.,0.));
#10194=DIRECTION('center_axis',(1.,0.,0.));
#10195=DIRECTION('ref_axis',(0.,0.,-1.));
#10196=DIRECTION('center_axis',(1.,0.,0.));
#10197=DIRECTION('ref_axis',(0.,2.68771689099506E-14,-1.));
#10198=DIRECTION('',(1.,3.30650148539799E-30,-1.22464679914735E-16));
#10199=DIRECTION('center_axis',(-1.,0.,0.));
#10200=DIRECTION('ref_axis',(0.,2.68771689099506E-14,-1.));
#10201=DIRECTION('center_axis',(1.,0.,0.));
#10202=DIRECTION('ref_axis',(0.,2.68771689099506E-14,-1.));
#10203=DIRECTION('',(1.,3.30650148539799E-30,-1.22464679914735E-16));
#10204=DIRECTION('center_axis',(1.,0.,0.));
#10205=DIRECTION('ref_axis',(0.,2.68771689099506E-14,-1.));
#10206=DIRECTION('',(1.,3.30650148539799E-30,-1.22464679914735E-16));
#10207=DIRECTION('center_axis',(1.,0.,0.));
#10208=DIRECTION('ref_axis',(0.,2.68771689099506E-14,-1.));
#10209=DIRECTION('',(1.,3.30650148539799E-30,-1.22464679914735E-16));
#10210=DIRECTION('center_axis',(1.,0.,0.));
#10211=DIRECTION('ref_axis',(0.,2.68771689099506E-14,-1.));
#10212=DIRECTION('',(1.,3.30650148539799E-30,-1.22464679914735E-16));
#10213=DIRECTION('center_axis',(1.,0.,0.));
#10214=DIRECTION('ref_axis',(0.,2.68771689099506E-14,-1.));
#10215=DIRECTION('',(1.,3.30650148539799E-30,-1.22464679914735E-16));
#10216=DIRECTION('center_axis',(1.,0.,0.));
#10217=DIRECTION('ref_axis',(0.,2.68771689099506E-14,-1.));
#10218=DIRECTION('',(1.,3.30650148539799E-30,-1.22464679914735E-16));
#10219=DIRECTION('center_axis',(1.,0.,0.));
#10220=DIRECTION('ref_axis',(0.,2.68771689099506E-14,-1.));
#10221=DIRECTION('',(1.,3.30650148539799E-30,-1.22464679914735E-16));
#10222=DIRECTION('center_axis',(1.,0.,0.));
#10223=DIRECTION('ref_axis',(0.,2.68771689099506E-14,-1.));
#10224=DIRECTION('',(1.,3.30650148539799E-30,-1.22464679914735E-16));
#10225=DIRECTION('center_axis',(1.,0.,0.));
#10226=DIRECTION('ref_axis',(0.,2.68771689099506E-14,-1.));
#10227=DIRECTION('center_axis',(1.,0.,0.));
#10228=DIRECTION('ref_axis',(0.,2.68771689099506E-14,-1.));
#10229=DIRECTION('center_axis',(1.,0.,0.));
#10230=DIRECTION('ref_axis',(0.,0.,-1.));
#10231=DIRECTION('',(0.,1.,0.));
#10232=DIRECTION('center_axis',(1.,0.,0.));
#10233=DIRECTION('ref_axis',(0.,0.,-1.));
#10234=DIRECTION('center_axis',(1.,0.,0.));
#10235=DIRECTION('ref_axis',(0.,0.,-1.));
#10236=DIRECTION('center_axis',(-1.,0.,0.));
#10237=DIRECTION('ref_axis',(0.,0.,-1.));
#10238=DIRECTION('center_axis',(-1.,0.,0.));
#10239=DIRECTION('ref_axis',(0.,0.,-1.));
#10240=DIRECTION('center_axis',(-1.,0.,0.));
#10241=DIRECTION('ref_axis',(0.,0.,-1.));
#10242=DIRECTION('center_axis',(1.,0.,0.));
#10243=DIRECTION('ref_axis',(0.,0.,-1.));
#10244=DIRECTION('center_axis',(1.,0.,0.));
#10245=DIRECTION('ref_axis',(0.,0.,-1.));
#10246=DIRECTION('',(1.,0.,0.));
#10247=DIRECTION('center_axis',(1.,0.,0.));
#10248=DIRECTION('ref_axis',(0.,0.,-1.));
#10249=DIRECTION('center_axis',(1.,0.,0.));
#10250=DIRECTION('ref_axis',(0.,0.,-1.));
#10251=DIRECTION('',(1.,0.,0.));
#10252=DIRECTION('center_axis',(1.,0.,0.));
#10253=DIRECTION('ref_axis',(0.,0.,-1.));
#10254=DIRECTION('center_axis',(1.,0.,0.));
#10255=DIRECTION('ref_axis',(0.,0.,-1.));
#10256=DIRECTION('',(1.,0.,0.));
#10257=DIRECTION('center_axis',(0.,0.,1.));
#10258=DIRECTION('ref_axis',(0.,-1.,0.));
#10259=DIRECTION('',(0.,-1.,0.));
#10260=DIRECTION('',(-1.,0.,0.));
#10261=DIRECTION('',(1.,0.,0.));
#10262=DIRECTION('center_axis',(1.,0.,0.));
#10263=DIRECTION('ref_axis',(0.,0.,-1.));
#10264=DIRECTION('center_axis',(1.,0.,0.));
#10265=DIRECTION('ref_axis',(0.,0.,-1.));
#10266=DIRECTION('center_axis',(1.,0.,0.));
#10267=DIRECTION('ref_axis',(0.,0.,-1.));
#10268=DIRECTION('center_axis',(1.,0.,0.));
#10269=DIRECTION('ref_axis',(0.,-1.22464679914735E-16,1.));
#10270=DIRECTION('center_axis',(1.,0.,0.));
#10271=DIRECTION('ref_axis',(0.,0.,-1.));
#10272=DIRECTION('center_axis',(1.,0.,0.));
#10273=DIRECTION('ref_axis',(0.,0.,-1.));
#10274=DIRECTION('',(-1.,0.,0.));
#10275=DIRECTION('center_axis',(1.,0.,0.));
#10276=DIRECTION('ref_axis',(0.,0.,-1.));
#10277=DIRECTION('center_axis',(1.,0.,0.));
#10278=DIRECTION('ref_axis',(0.,0.,-1.));
#10279=DIRECTION('axis',(0.,0.,1.));
#10280=DIRECTION('refdir',(1.,0.,0.));
#10281=DIRECTION('center_axis',(0.,1.,0.));
#10282=DIRECTION('ref_axis',(0.,0.,1.));
#10283=DIRECTION('center_axis',(0.,-1.,0.));
#10284=DIRECTION('ref_axis',(1.,0.,0.));
#10285=DIRECTION('center_axis',(0.,-1.,0.));
#10286=DIRECTION('ref_axis',(1.,0.,0.));
#10287=DIRECTION('center_axis',(0.,-1.,0.));
#10288=DIRECTION('ref_axis',(1.,0.,0.));
#10289=DIRECTION('',(0.707106781186548,0.707106781186547,8.65956056235493E-17));
#10290=DIRECTION('center_axis',(0.,-1.,0.));
#10291=DIRECTION('ref_axis',(1.,0.,0.));
#10292=DIRECTION('center_axis',(0.,-1.,0.));
#10293=DIRECTION('ref_axis',(1.,0.,0.));
#10294=DIRECTION('',(0.,1.,0.));
#10295=DIRECTION('center_axis',(0.,1.,0.));
#10296=DIRECTION('ref_axis',(1.,0.,0.));
#10297=DIRECTION('center_axis',(0.,-1.,0.));
#10298=DIRECTION('ref_axis',(1.,0.,0.));
#10299=DIRECTION('',(-0.707106781186547,0.707106781186548,-8.65956056235493E-17));
#10300=DIRECTION('center_axis',(0.,-1.,0.));
#10301=DIRECTION('ref_axis',(0.,0.,-1.));
#10302=DIRECTION('center_axis',(0.,-1.,0.));
#10303=DIRECTION('ref_axis',(1.,0.,0.));
#10304=DIRECTION('center_axis',(0.,1.,0.));
#10305=DIRECTION('ref_axis',(1.,0.,0.));
#10306=DIRECTION('center_axis',(0.,1.,0.));
#10307=DIRECTION('ref_axis',(1.,0.,0.));
#10308=DIRECTION('',(-0.447213595499958,0.894427190999916,-5.47678698264203E-17));
#10309=DIRECTION('center_axis',(0.,-1.,0.));
#10310=DIRECTION('ref_axis',(1.,0.,0.));
#10311=DIRECTION('center_axis',(0.,1.,0.));
#10312=DIRECTION('ref_axis',(1.,0.,0.));
#10313=DIRECTION('',(0.,1.,0.));
#10314=DIRECTION('center_axis',(0.,1.,0.));
#10315=DIRECTION('ref_axis',(1.,0.,0.));
#10316=DIRECTION('center_axis',(0.,-1.,0.));
#10317=DIRECTION('ref_axis',(1.,0.,0.));
#10318=DIRECTION('',(-0.707106781186547,0.707106781186548,-8.65956056235493E-17));
#10319=DIRECTION('center_axis',(0.,-1.,0.));
#10320=DIRECTION('ref_axis',(0.,0.,-1.));
#10321=DIRECTION('center_axis',(0.866025403784439,0.,-0.5));
#10322=DIRECTION('ref_axis',(0.5,0.,0.866025403784439));
#10323=DIRECTION('',(-0.5,0.,-0.866025403784439));
#10324=DIRECTION('',(0.,-1.,0.));
#10325=DIRECTION('',(0.5,0.,0.866025403784439));
#10326=DIRECTION('',(0.,-1.,0.));
#10327=DIRECTION('center_axis',(1.20185167898973E-16,0.,-1.));
#10328=DIRECTION('ref_axis',(1.,0.,1.20185167898973E-16));
#10329=DIRECTION('',(-1.,0.,-1.20185167898973E-16));
#10330=DIRECTION('',(0.,-1.,0.));
#10331=DIRECTION('',(1.,0.,1.20185167898973E-16));
#10332=DIRECTION('center_axis',(-0.866025403784439,0.,-0.5));
#10333=DIRECTION('ref_axis',(0.5,0.,-0.866025403784439));
#10334=DIRECTION('',(-0.5,0.,0.866025403784439));
#10335=DIRECTION('',(0.,-1.,0.));
#10336=DIRECTION('',(0.5,0.,-0.866025403784439));
#10337=DIRECTION('center_axis',(-0.866025403784439,0.,0.5));
#10338=DIRECTION('ref_axis',(-0.5,0.,-0.866025403784439));
#10339=DIRECTION('',(0.5,0.,0.866025403784439));
#10340=DIRECTION('',(0.,-1.,0.));
#10341=DIRECTION('',(-0.5,0.,-0.866025403784439));
#10342=DIRECTION('center_axis',(-2.40370335797945E-16,0.,1.));
#10343=DIRECTION('ref_axis',(-1.,0.,-2.40370335797945E-16));
#10344=DIRECTION('',(1.,0.,2.40370335797945E-16));
#10345=DIRECTION('',(0.,-1.,0.));
#10346=DIRECTION('',(-1.,0.,-2.40370335797945E-16));
#10347=DIRECTION('center_axis',(0.866025403784439,0.,0.5));
#10348=DIRECTION('ref_axis',(-0.5,0.,0.866025403784439));
#10349=DIRECTION('',(0.5,0.,-0.866025403784439));
#10350=DIRECTION('',(-0.5,0.,0.866025403784439));
#10351=DIRECTION('center_axis',(0.,1.,0.));
#10352=DIRECTION('ref_axis',(1.,0.,0.));
#10353=DIRECTION('center_axis',(0.,-1.,0.));
#10354=DIRECTION('ref_axis',(0.,0.,-1.));
#10355=DIRECTION('axis',(0.,0.,1.));
#10356=DIRECTION('refdir',(1.,0.,0.));
#10357=DIRECTION('center_axis',(0.,1.,0.));
#10358=DIRECTION('ref_axis',(0.,0.,1.));
#10359=DIRECTION('center_axis',(0.,-1.,0.));
#10360=DIRECTION('ref_axis',(1.,0.,0.));
#10361=DIRECTION('center_axis',(0.,-1.,0.));
#10362=DIRECTION('ref_axis',(1.,0.,0.));
#10363=DIRECTION('center_axis',(0.,-1.,0.));
#10364=DIRECTION('ref_axis',(1.,0.,0.));
#10365=DIRECTION('',(0.707106781186547,0.707106781186548,8.65956056235493E-17));
#10366=DIRECTION('center_axis',(0.,-1.,0.));
#10367=DIRECTION('ref_axis',(1.,0.,0.));
#10368=DIRECTION('center_axis',(0.,-1.,0.));
#10369=DIRECTION('ref_axis',(1.,0.,0.));
#10370=DIRECTION('',(0.,1.,0.));
#10371=DIRECTION('center_axis',(0.,1.,0.));
#10372=DIRECTION('ref_axis',(1.,0.,0.));
#10373=DIRECTION('center_axis',(0.,-1.,0.));
#10374=DIRECTION('ref_axis',(1.,0.,0.));
#10375=DIRECTION('',(-0.707106781186547,0.707106781186548,-8.65956056235493E-17));
#10376=DIRECTION('center_axis',(0.,-1.,0.));
#10377=DIRECTION('ref_axis',(0.,0.,-1.));
#10378=DIRECTION('center_axis',(0.,-1.,0.));
#10379=DIRECTION('ref_axis',(1.,0.,0.));
#10380=DIRECTION('center_axis',(0.,1.,0.));
#10381=DIRECTION('ref_axis',(1.,0.,0.));
#10382=DIRECTION('center_axis',(0.,1.,0.));
#10383=DIRECTION('ref_axis',(1.,0.,0.));
#10384=DIRECTION('',(-0.447213595499958,0.894427190999916,-5.47678698264203E-17));
#10385=DIRECTION('center_axis',(0.,-1.,0.));
#10386=DIRECTION('ref_axis',(1.,0.,0.));
#10387=DIRECTION('center_axis',(0.,1.,0.));
#10388=DIRECTION('ref_axis',(1.,0.,0.));
#10389=DIRECTION('',(0.,1.,0.));
#10390=DIRECTION('center_axis',(0.,1.,0.));
#10391=DIRECTION('ref_axis',(1.,0.,0.));
#10392=DIRECTION('center_axis',(0.,-1.,0.));
#10393=DIRECTION('ref_axis',(1.,0.,0.));
#10394=DIRECTION('',(-0.707106781186547,0.707106781186548,-8.65956056235493E-17));
#10395=DIRECTION('center_axis',(0.,-1.,0.));
#10396=DIRECTION('ref_axis',(0.,0.,-1.));
#10397=DIRECTION('center_axis',(0.866025403784439,0.,-0.5));
#10398=DIRECTION('ref_axis',(0.5,0.,0.866025403784439));
#10399=DIRECTION('',(-0.5,0.,-0.866025403784439));
#10400=DIRECTION('',(0.,-1.,0.));
#10401=DIRECTION('',(0.5,0.,0.866025403784439));
#10402=DIRECTION('',(0.,-1.,0.));
#10403=DIRECTION('center_axis',(1.60246890531964E-16,0.,-1.));
#10404=DIRECTION('ref_axis',(1.,0.,1.60246890531964E-16));
#10405=DIRECTION('',(-1.,0.,-1.60246890531964E-16));
#10406=DIRECTION('',(0.,-1.,0.));
#10407=DIRECTION('',(1.,0.,1.60246890531964E-16));
#10408=DIRECTION('center_axis',(-0.866025403784439,0.,-0.5));
#10409=DIRECTION('ref_axis',(0.5,0.,-0.866025403784439));
#10410=DIRECTION('',(-0.5,0.,0.866025403784439));
#10411=DIRECTION('',(0.,-1.,0.));
#10412=DIRECTION('',(0.5,0.,-0.866025403784439));
#10413=DIRECTION('center_axis',(-0.866025403784439,0.,0.5));
#10414=DIRECTION('ref_axis',(-0.5,0.,-0.866025403784439));
#10415=DIRECTION('',(0.5,0.,0.866025403784439));
#10416=DIRECTION('',(0.,-1.,0.));
#10417=DIRECTION('',(-0.5,0.,-0.866025403784439));
#10418=DIRECTION('center_axis',(-1.60246890531964E-16,0.,1.));
#10419=DIRECTION('ref_axis',(-1.,0.,-1.60246890531964E-16));
#10420=DIRECTION('',(1.,0.,1.60246890531964E-16));
#10421=DIRECTION('',(0.,-1.,0.));
#10422=DIRECTION('',(-1.,0.,-1.60246890531964E-16));
#10423=DIRECTION('center_axis',(0.866025403784439,0.,0.5));
#10424=DIRECTION('ref_axis',(-0.5,0.,0.866025403784439));
#10425=DIRECTION('',(0.5,0.,-0.866025403784439));
#10426=DIRECTION('',(-0.5,0.,0.866025403784439));
#10427=DIRECTION('center_axis',(0.,1.,0.));
#10428=DIRECTION('ref_axis',(1.,0.,0.));
#10429=DIRECTION('center_axis',(0.,-1.,0.));
#10430=DIRECTION('ref_axis',(0.,0.,-1.));
#10431=DIRECTION('',(0.,0.,1.));
#10432=DIRECTION('',(1.,0.,0.));
#10433=DIRECTION('',(0.,0.,1.));
#10434=DIRECTION('',(1.,0.,0.));
#10435=DIRECTION('',(0.,0.,1.));
#10436=DIRECTION('',(1.,0.,0.));
#10437=DIRECTION('',(0.,0.,1.));
#10438=DIRECTION('',(1.,0.,0.));
#10439=DIRECTION('',(0.,0.,1.));
#10440=DIRECTION('',(1.,0.,0.));
#10441=DIRECTION('',(0.,0.,1.));
#10442=DIRECTION('',(1.,0.,0.));
#10443=DIRECTION('',(0.,0.,1.));
#10444=DIRECTION('',(2.22044604925031E-16,1.,0.));
#10445=DIRECTION('',(0.,0.,1.));
#10446=DIRECTION('',(2.22044604925031E-16,1.,0.));
#10447=DIRECTION('',(0.,0.,1.));
#10448=DIRECTION('',(2.22044604925031E-16,-1.,0.));
#10449=DIRECTION('',(0.,0.,1.));
#10450=DIRECTION('',(2.22044604925031E-16,-1.,0.));
#10451=DIRECTION('',(0.,0.,1.));
#10452=DIRECTION('',(2.22044604925031E-16,-1.,0.));
#10453=DIRECTION('axis',(0.,0.,1.));
#10454=DIRECTION('refdir',(1.,0.,0.));
#10455=DIRECTION('axis',(0.,0.,1.));
#10456=DIRECTION('refdir',(1.,0.,0.));
#10457=DIRECTION('center_axis',(1.,0.,0.));
#10458=DIRECTION('ref_axis',(0.,0.975560628713931,0.219730425074181));
#10459=DIRECTION('',(-1.,0.,0.));
#10460=DIRECTION('center_axis',(-1.,0.,0.));
#10461=DIRECTION('ref_axis',(0.,0.,-1.));
#10462=DIRECTION('center_axis',(1.,0.,0.));
#10463=DIRECTION('ref_axis',(0.,0.,-1.));
#10464=DIRECTION('',(-1.,0.,0.));
#10465=DIRECTION('center_axis',(1.,0.,0.));
#10466=DIRECTION('ref_axis',(0.,0.,-1.));
#10467=DIRECTION('',(-1.,0.,0.));
#10468=DIRECTION('center_axis',(1.,0.,0.));
#10469=DIRECTION('ref_axis',(0.,0.,-1.));
#10470=DIRECTION('',(-1.,0.,0.));
#10471=DIRECTION('center_axis',(1.,0.,0.));
#10472=DIRECTION('ref_axis',(0.,0.,-1.));
#10473=DIRECTION('',(-1.,0.,0.));
#10474=DIRECTION('center_axis',(1.,0.,0.));
#10475=DIRECTION('ref_axis',(0.,0.,-1.));
#10476=DIRECTION('',(-1.,0.,0.));
#10477=DIRECTION('center_axis',(1.,0.,0.));
#10478=DIRECTION('ref_axis',(0.,0.,-1.));
#10479=DIRECTION('',(-1.,0.,0.));
#10480=DIRECTION('center_axis',(1.,0.,0.));
#10481=DIRECTION('ref_axis',(0.,0.,-1.));
#10482=DIRECTION('',(-1.,0.,0.));
#10483=DIRECTION('center_axis',(1.,0.,0.));
#10484=DIRECTION('ref_axis',(0.,0.,-1.));
#10485=DIRECTION('',(-1.,0.,0.));
#10486=DIRECTION('center_axis',(1.,0.,0.));
#10487=DIRECTION('ref_axis',(0.,0.,-1.));
#10488=DIRECTION('',(-1.,0.,0.));
#10489=DIRECTION('center_axis',(1.,0.,0.));
#10490=DIRECTION('ref_axis',(0.,0.,-1.));
#10491=DIRECTION('',(-1.,0.,0.));
#10492=DIRECTION('center_axis',(1.,0.,0.));
#10493=DIRECTION('ref_axis',(0.,0.,-1.));
#10494=DIRECTION('',(-1.,0.,0.));
#10495=DIRECTION('center_axis',(1.,0.,0.));
#10496=DIRECTION('ref_axis',(0.,0.,-1.));
#10497=DIRECTION('',(-1.,0.,0.));
#10498=DIRECTION('center_axis',(1.,0.,0.));
#10499=DIRECTION('ref_axis',(0.,0.,-1.));
#10500=DIRECTION('',(-1.,0.,0.));
#10501=DIRECTION('center_axis',(1.,0.,0.));
#10502=DIRECTION('ref_axis',(0.,0.,-1.));
#10503=DIRECTION('',(-1.,0.,0.));
#10504=DIRECTION('center_axis',(1.,0.,0.));
#10505=DIRECTION('ref_axis',(0.,0.,-1.));
#10506=DIRECTION('',(-1.,0.,0.));
#10507=DIRECTION('center_axis',(1.,0.,0.));
#10508=DIRECTION('ref_axis',(0.,0.,-1.));
#10509=DIRECTION('',(-1.,0.,0.));
#10510=DIRECTION('center_axis',(1.,0.,0.));
#10511=DIRECTION('ref_axis',(0.,0.,-1.));
#10512=DIRECTION('',(-1.,0.,0.));
#10513=DIRECTION('center_axis',(1.,0.,0.));
#10514=DIRECTION('ref_axis',(0.,0.,-1.));
#10515=DIRECTION('',(-1.,0.,0.));
#10516=DIRECTION('center_axis',(1.,0.,0.));
#10517=DIRECTION('ref_axis',(0.,0.,-1.));
#10518=DIRECTION('',(-1.,0.,0.));
#10519=DIRECTION('center_axis',(1.,0.,0.));
#10520=DIRECTION('ref_axis',(0.,0.,-1.));
#10521=DIRECTION('',(-1.,0.,0.));
#10522=DIRECTION('center_axis',(1.,0.,0.));
#10523=DIRECTION('ref_axis',(0.,0.,-1.));
#10524=DIRECTION('',(-1.,0.,0.));
#10525=DIRECTION('center_axis',(1.,0.,0.));
#10526=DIRECTION('ref_axis',(0.,0.,-1.));
#10527=DIRECTION('',(-1.,0.,0.));
#10528=DIRECTION('center_axis',(1.,0.,0.));
#10529=DIRECTION('ref_axis',(0.,0.,-1.));
#10530=DIRECTION('',(-1.,0.,0.));
#10531=DIRECTION('center_axis',(1.,0.,0.));
#10532=DIRECTION('ref_axis',(0.,0.,-1.));
#10533=DIRECTION('',(-1.,0.,0.));
#10534=DIRECTION('center_axis',(1.,0.,0.));
#10535=DIRECTION('ref_axis',(0.,0.,-1.));
#10536=DIRECTION('',(-1.,0.,0.));
#10537=DIRECTION('center_axis',(1.,0.,0.));
#10538=DIRECTION('ref_axis',(0.,0.,-1.));
#10539=DIRECTION('',(-1.,0.,0.));
#10540=DIRECTION('center_axis',(1.,0.,0.));
#10541=DIRECTION('ref_axis',(0.,0.,-1.));
#10542=DIRECTION('',(-1.,0.,0.));
#10543=DIRECTION('center_axis',(1.,0.,0.));
#10544=DIRECTION('ref_axis',(0.,0.,-1.));
#10545=DIRECTION('',(-1.,0.,0.));
#10546=DIRECTION('center_axis',(1.,0.,0.));
#10547=DIRECTION('ref_axis',(0.,0.,-1.));
#10548=DIRECTION('',(-1.,0.,0.));
#10549=DIRECTION('center_axis',(1.,0.,0.));
#10550=DIRECTION('ref_axis',(0.,0.,-1.));
#10551=DIRECTION('',(-1.,0.,0.));
#10552=DIRECTION('center_axis',(1.,0.,0.));
#10553=DIRECTION('ref_axis',(0.,0.,-1.));
#10554=DIRECTION('',(-1.,0.,0.));
#10555=DIRECTION('center_axis',(1.,0.,0.));
#10556=DIRECTION('ref_axis',(0.,0.,-1.));
#10557=DIRECTION('',(-1.,0.,0.));
#10558=DIRECTION('center_axis',(1.,0.,0.));
#10559=DIRECTION('ref_axis',(0.,0.,-1.));
#10560=DIRECTION('',(-1.,0.,0.));
#10561=DIRECTION('center_axis',(1.,0.,0.));
#10562=DIRECTION('ref_axis',(0.,0.,-1.));
#10563=DIRECTION('',(-1.,0.,0.));
#10564=DIRECTION('center_axis',(1.,0.,0.));
#10565=DIRECTION('ref_axis',(0.,0.,-1.));
#10566=DIRECTION('',(-1.,0.,0.));
#10567=DIRECTION('center_axis',(1.,0.,0.));
#10568=DIRECTION('ref_axis',(0.,0.,-1.));
#10569=DIRECTION('',(-1.,0.,0.));
#10570=DIRECTION('center_axis',(1.,0.,0.));
#10571=DIRECTION('ref_axis',(0.,0.,-1.));
#10572=DIRECTION('',(-1.,0.,0.));
#10573=DIRECTION('center_axis',(1.,0.,0.));
#10574=DIRECTION('ref_axis',(0.,0.,-1.));
#10575=DIRECTION('',(-1.,0.,0.));
#10576=DIRECTION('center_axis',(1.,0.,0.));
#10577=DIRECTION('ref_axis',(0.,0.,-1.));
#10578=DIRECTION('',(-1.,0.,0.));
#10579=DIRECTION('center_axis',(1.,0.,0.));
#10580=DIRECTION('ref_axis',(0.,0.,-1.));
#10581=DIRECTION('',(-1.,0.,0.));
#10582=DIRECTION('center_axis',(1.,0.,0.));
#10583=DIRECTION('ref_axis',(0.,0.,-1.));
#10584=DIRECTION('',(-1.,0.,0.));
#10585=DIRECTION('center_axis',(1.,0.,0.));
#10586=DIRECTION('ref_axis',(0.,0.,-1.));
#10587=DIRECTION('',(-1.,0.,0.));
#10588=DIRECTION('center_axis',(1.,0.,0.));
#10589=DIRECTION('ref_axis',(0.,0.,-1.));
#10590=DIRECTION('',(-1.,0.,0.));
#10591=DIRECTION('center_axis',(1.,0.,0.));
#10592=DIRECTION('ref_axis',(0.,0.,-1.));
#10593=DIRECTION('',(-1.,0.,0.));
#10594=DIRECTION('center_axis',(1.,0.,0.));
#10595=DIRECTION('ref_axis',(0.,0.,-1.));
#10596=DIRECTION('',(-1.,0.,0.));
#10597=DIRECTION('center_axis',(1.,0.,0.));
#10598=DIRECTION('ref_axis',(0.,0.,-1.));
#10599=DIRECTION('',(-1.,0.,0.));
#10600=DIRECTION('center_axis',(1.,0.,0.));
#10601=DIRECTION('ref_axis',(0.,0.,-1.));
#10602=DIRECTION('',(-1.,0.,0.));
#10603=DIRECTION('center_axis',(1.,0.,0.));
#10604=DIRECTION('ref_axis',(0.,0.,-1.));
#10605=DIRECTION('',(-1.,0.,0.));
#10606=DIRECTION('center_axis',(1.,0.,0.));
#10607=DIRECTION('ref_axis',(0.,0.,-1.));
#10608=DIRECTION('',(-1.,0.,0.));
#10609=DIRECTION('center_axis',(1.,0.,0.));
#10610=DIRECTION('ref_axis',(0.,0.,-1.));
#10611=DIRECTION('',(-1.,0.,0.));
#10612=DIRECTION('center_axis',(1.,0.,0.));
#10613=DIRECTION('ref_axis',(0.,0.,-1.));
#10614=DIRECTION('',(-1.,0.,0.));
#10615=DIRECTION('center_axis',(1.,0.,0.));
#10616=DIRECTION('ref_axis',(0.,0.,-1.));
#10617=DIRECTION('',(-1.,0.,0.));
#10618=DIRECTION('center_axis',(1.,0.,0.));
#10619=DIRECTION('ref_axis',(0.,0.,-1.));
#10620=DIRECTION('',(-1.,0.,0.));
#10621=DIRECTION('center_axis',(1.,0.,0.));
#10622=DIRECTION('ref_axis',(0.,0.,-1.));
#10623=DIRECTION('',(-1.,0.,0.));
#10624=DIRECTION('center_axis',(1.,0.,0.));
#10625=DIRECTION('ref_axis',(0.,0.,-1.));
#10626=DIRECTION('',(-1.,0.,0.));
#10627=DIRECTION('center_axis',(1.,0.,0.));
#10628=DIRECTION('ref_axis',(0.,0.,-1.));
#10629=DIRECTION('',(-1.,0.,0.));
#10630=DIRECTION('center_axis',(1.,0.,0.));
#10631=DIRECTION('ref_axis',(0.,0.,-1.));
#10632=DIRECTION('',(-1.,0.,0.));
#10633=DIRECTION('center_axis',(1.,0.,0.));
#10634=DIRECTION('ref_axis',(0.,0.,-1.));
#10635=DIRECTION('',(-1.,0.,0.));
#10636=DIRECTION('center_axis',(1.,0.,0.));
#10637=DIRECTION('ref_axis',(0.,0.,-1.));
#10638=DIRECTION('',(-1.,0.,0.));
#10639=DIRECTION('center_axis',(1.,0.,0.));
#10640=DIRECTION('ref_axis',(0.,0.,-1.));
#10641=DIRECTION('',(-1.,0.,0.));
#10642=DIRECTION('center_axis',(1.,0.,0.));
#10643=DIRECTION('ref_axis',(0.,0.,-1.));
#10644=DIRECTION('',(-1.,0.,0.));
#10645=DIRECTION('center_axis',(1.,0.,0.));
#10646=DIRECTION('ref_axis',(0.,0.,-1.));
#10647=DIRECTION('',(-1.,0.,0.));
#10648=DIRECTION('center_axis',(1.,0.,0.));
#10649=DIRECTION('ref_axis',(0.,-1.17203152359781E-12,-1.));
#10650=DIRECTION('',(1.,0.,0.));
#10651=DIRECTION('center_axis',(1.,0.,0.));
#10652=DIRECTION('ref_axis',(0.,-1.17203152359781E-12,-1.));
#10653=DIRECTION('center_axis',(1.,0.,0.));
#10654=DIRECTION('ref_axis',(0.,-1.17203152359781E-12,-1.));
#10655=DIRECTION('',(1.,0.,0.));
#10656=DIRECTION('center_axis',(1.,0.,0.));
#10657=DIRECTION('ref_axis',(0.,-1.17203152359781E-12,-1.));
#10658=DIRECTION('center_axis',(1.,0.,0.));
#10659=DIRECTION('ref_axis',(0.,-1.17203152359781E-12,-1.));
#10660=DIRECTION('',(1.,0.,0.));
#10661=DIRECTION('center_axis',(1.,0.,0.));
#10662=DIRECTION('ref_axis',(0.,-1.17203152359781E-12,-1.));
#10663=DIRECTION('',(1.,0.,0.));
#10664=DIRECTION('center_axis',(1.,0.,0.));
#10665=DIRECTION('ref_axis',(0.,-1.17203152359781E-12,-1.));
#10666=DIRECTION('',(1.,0.,0.));
#10667=DIRECTION('center_axis',(1.,0.,0.));
#10668=DIRECTION('ref_axis',(0.,-1.17203152359781E-12,-1.));
#10669=DIRECTION('',(1.,0.,0.));
#10670=DIRECTION('center_axis',(1.,0.,0.));
#10671=DIRECTION('ref_axis',(0.,-1.17203152359781E-12,-1.));
#10672=DIRECTION('',(1.,0.,0.));
#10673=DIRECTION('center_axis',(1.,0.,0.));
#10674=DIRECTION('ref_axis',(0.,-1.17203152359781E-12,-1.));
#10675=DIRECTION('',(1.,0.,0.));
#10676=DIRECTION('center_axis',(1.,0.,0.));
#10677=DIRECTION('ref_axis',(0.,-1.17203152359781E-12,-1.));
#10678=DIRECTION('',(1.,0.,0.));
#10679=DIRECTION('center_axis',(1.,0.,0.));
#10680=DIRECTION('ref_axis',(0.,-1.17203152359781E-12,-1.));
#10681=DIRECTION('',(1.,0.,0.));
#10682=DIRECTION('center_axis',(1.,0.,0.));
#10683=DIRECTION('ref_axis',(0.,-1.17203152359781E-12,-1.));
#10684=DIRECTION('',(1.,0.,0.));
#10685=DIRECTION('center_axis',(1.,0.,0.));
#10686=DIRECTION('ref_axis',(0.,-1.17203152359781E-12,-1.));
#10687=DIRECTION('',(1.,0.,0.));
#10688=DIRECTION('center_axis',(1.,0.,0.));
#10689=DIRECTION('ref_axis',(0.,-1.17203152359781E-12,-1.));
#10690=DIRECTION('',(1.,0.,0.));
#10691=DIRECTION('center_axis',(1.,0.,0.));
#10692=DIRECTION('ref_axis',(0.,-1.17203152359781E-12,-1.));
#10693=DIRECTION('',(1.,0.,0.));
#10694=DIRECTION('center_axis',(1.,0.,0.));
#10695=DIRECTION('ref_axis',(0.,-1.17203152359781E-12,-1.));
#10696=DIRECTION('',(1.,0.,0.));
#10697=DIRECTION('center_axis',(1.,0.,0.));
#10698=DIRECTION('ref_axis',(0.,-1.17203152359781E-12,-1.));
#10699=DIRECTION('',(1.,0.,0.));
#10700=DIRECTION('center_axis',(1.,0.,0.));
#10701=DIRECTION('ref_axis',(0.,-1.17203152359781E-12,-1.));
#10702=DIRECTION('',(1.,0.,0.));
#10703=DIRECTION('center_axis',(1.,0.,0.));
#10704=DIRECTION('ref_axis',(0.,-1.17203152359781E-12,-1.));
#10705=DIRECTION('',(1.,0.,0.));
#10706=DIRECTION('center_axis',(1.,0.,0.));
#10707=DIRECTION('ref_axis',(0.,-1.17203152359781E-12,-1.));
#10708=DIRECTION('',(1.,0.,0.));
#10709=DIRECTION('center_axis',(1.,0.,0.));
#10710=DIRECTION('ref_axis',(0.,-1.17203152359781E-12,-1.));
#10711=DIRECTION('',(1.,0.,0.));
#10712=DIRECTION('center_axis',(1.,0.,0.));
#10713=DIRECTION('ref_axis',(0.,-1.17203152359781E-12,-1.));
#10714=DIRECTION('',(1.,0.,0.));
#10715=DIRECTION('center_axis',(1.,0.,0.));
#10716=DIRECTION('ref_axis',(0.,-1.17203152359781E-12,-1.));
#10717=DIRECTION('',(1.,0.,0.));
#10718=DIRECTION('center_axis',(1.,0.,0.));
#10719=DIRECTION('ref_axis',(0.,-1.17203152359781E-12,-1.));
#10720=DIRECTION('',(1.,0.,0.));
#10721=DIRECTION('center_axis',(1.,0.,0.));
#10722=DIRECTION('ref_axis',(0.,-1.17203152359781E-12,-1.));
#10723=DIRECTION('',(1.,0.,0.));
#10724=DIRECTION('center_axis',(1.,0.,0.));
#10725=DIRECTION('ref_axis',(0.,-1.17203152359781E-12,-1.));
#10726=DIRECTION('',(1.,0.,0.));
#10727=DIRECTION('center_axis',(1.,0.,0.));
#10728=DIRECTION('ref_axis',(0.,-1.17203152359781E-12,-1.));
#10729=DIRECTION('',(1.,0.,0.));
#10730=DIRECTION('center_axis',(1.,0.,0.));
#10731=DIRECTION('ref_axis',(0.,-1.17203152359781E-12,-1.));
#10732=DIRECTION('',(1.,0.,0.));
#10733=DIRECTION('center_axis',(1.,0.,0.));
#10734=DIRECTION('ref_axis',(0.,-1.17203152359781E-12,-1.));
#10735=DIRECTION('',(1.,0.,0.));
#10736=DIRECTION('center_axis',(1.,0.,0.));
#10737=DIRECTION('ref_axis',(0.,-1.17203152359781E-12,-1.));
#10738=DIRECTION('',(1.,0.,0.));
#10739=DIRECTION('center_axis',(1.,0.,0.));
#10740=DIRECTION('ref_axis',(0.,-1.17203152359781E-12,-1.));
#10741=DIRECTION('',(1.,0.,0.));
#10742=DIRECTION('center_axis',(1.,0.,0.));
#10743=DIRECTION('ref_axis',(0.,-1.17203152359781E-12,-1.));
#10744=DIRECTION('',(1.,0.,0.));
#10745=DIRECTION('center_axis',(1.,0.,0.));
#10746=DIRECTION('ref_axis',(0.,-1.17203152359781E-12,-1.));
#10747=DIRECTION('',(1.,0.,0.));
#10748=DIRECTION('center_axis',(1.,0.,0.));
#10749=DIRECTION('ref_axis',(0.,-1.17203152359781E-12,-1.));
#10750=DIRECTION('',(1.,0.,0.));
#10751=DIRECTION('center_axis',(1.,0.,0.));
#10752=DIRECTION('ref_axis',(0.,-1.17203152359781E-12,-1.));
#10753=DIRECTION('',(1.,0.,0.));
#10754=DIRECTION('center_axis',(1.,0.,0.));
#10755=DIRECTION('ref_axis',(0.,-1.17203152359781E-12,-1.));
#10756=DIRECTION('',(1.,0.,0.));
#10757=DIRECTION('center_axis',(1.,0.,0.));
#10758=DIRECTION('ref_axis',(0.,-1.17203152359781E-12,-1.));
#10759=DIRECTION('',(1.,0.,0.));
#10760=DIRECTION('center_axis',(1.,0.,0.));
#10761=DIRECTION('ref_axis',(0.,-1.17203152359781E-12,-1.));
#10762=DIRECTION('',(1.,0.,0.));
#10763=DIRECTION('center_axis',(1.,0.,0.));
#10764=DIRECTION('ref_axis',(0.,-1.17203152359781E-12,-1.));
#10765=DIRECTION('',(1.,0.,0.));
#10766=DIRECTION('center_axis',(1.,0.,0.));
#10767=DIRECTION('ref_axis',(0.,-1.17203152359781E-12,-1.));
#10768=DIRECTION('',(1.,0.,0.));
#10769=DIRECTION('center_axis',(1.,0.,0.));
#10770=DIRECTION('ref_axis',(0.,-1.17203152359781E-12,-1.));
#10771=DIRECTION('',(1.,0.,0.));
#10772=DIRECTION('center_axis',(1.,0.,0.));
#10773=DIRECTION('ref_axis',(0.,-1.17203152359781E-12,-1.));
#10774=DIRECTION('',(1.,0.,0.));
#10775=DIRECTION('center_axis',(1.,0.,0.));
#10776=DIRECTION('ref_axis',(0.,-1.17203152359781E-12,-1.));
#10777=DIRECTION('',(1.,0.,0.));
#10778=DIRECTION('center_axis',(1.,0.,0.));
#10779=DIRECTION('ref_axis',(0.,-1.17203152359781E-12,-1.));
#10780=DIRECTION('',(1.,0.,0.));
#10781=DIRECTION('center_axis',(1.,0.,0.));
#10782=DIRECTION('ref_axis',(0.,-1.17203152359781E-12,-1.));
#10783=DIRECTION('',(1.,0.,0.));
#10784=DIRECTION('center_axis',(1.,0.,0.));
#10785=DIRECTION('ref_axis',(0.,-1.17203152359781E-12,-1.));
#10786=DIRECTION('',(1.,0.,0.));
#10787=DIRECTION('center_axis',(1.,0.,0.));
#10788=DIRECTION('ref_axis',(0.,-1.17203152359781E-12,-1.));
#10789=DIRECTION('',(1.,0.,0.));
#10790=DIRECTION('center_axis',(1.,0.,0.));
#10791=DIRECTION('ref_axis',(0.,-1.17203152359781E-12,-1.));
#10792=DIRECTION('',(1.,0.,0.));
#10793=DIRECTION('center_axis',(1.,0.,0.));
#10794=DIRECTION('ref_axis',(0.,-1.17203152359781E-12,-1.));
#10795=DIRECTION('',(1.,0.,0.));
#10796=DIRECTION('center_axis',(1.,0.,0.));
#10797=DIRECTION('ref_axis',(0.,-1.17203152359781E-12,-1.));
#10798=DIRECTION('',(1.,0.,0.));
#10799=DIRECTION('center_axis',(1.,0.,0.));
#10800=DIRECTION('ref_axis',(0.,-1.17203152359781E-12,-1.));
#10801=DIRECTION('',(1.,0.,0.));
#10802=DIRECTION('center_axis',(1.,0.,0.));
#10803=DIRECTION('ref_axis',(0.,-1.17203152359781E-12,-1.));
#10804=DIRECTION('',(1.,0.,0.));
#10805=DIRECTION('center_axis',(1.,0.,0.));
#10806=DIRECTION('ref_axis',(0.,-1.17203152359781E-12,-1.));
#10807=DIRECTION('',(1.,0.,0.));
#10808=DIRECTION('center_axis',(1.,0.,0.));
#10809=DIRECTION('ref_axis',(0.,-1.17203152359781E-12,-1.));
#10810=DIRECTION('',(1.,0.,0.));
#10811=DIRECTION('center_axis',(1.,0.,0.));
#10812=DIRECTION('ref_axis',(0.,-1.17203152359781E-12,-1.));
#10813=DIRECTION('',(1.,0.,0.));
#10814=DIRECTION('center_axis',(1.,0.,0.));
#10815=DIRECTION('ref_axis',(0.,-1.17203152359781E-12,-1.));
#10816=DIRECTION('',(1.,0.,0.));
#10817=DIRECTION('center_axis',(1.,0.,0.));
#10818=DIRECTION('ref_axis',(0.,-1.17203152359781E-12,-1.));
#10819=DIRECTION('',(1.,0.,0.));
#10820=DIRECTION('center_axis',(1.,0.,0.));
#10821=DIRECTION('ref_axis',(0.,-1.17203152359781E-12,-1.));
#10822=DIRECTION('',(1.,0.,0.));
#10823=DIRECTION('center_axis',(1.,0.,0.));
#10824=DIRECTION('ref_axis',(0.,-1.17203152359781E-12,-1.));
#10825=DIRECTION('',(1.,0.,0.));
#10826=DIRECTION('center_axis',(1.,0.,0.));
#10827=DIRECTION('ref_axis',(0.,-1.17203152359781E-12,-1.));
#10828=DIRECTION('',(1.,0.,0.));
#10829=DIRECTION('center_axis',(1.,0.,0.));
#10830=DIRECTION('ref_axis',(0.,-1.17203152359781E-12,-1.));
#10831=DIRECTION('',(1.,0.,0.));
#10832=DIRECTION('center_axis',(1.,0.,0.));
#10833=DIRECTION('ref_axis',(0.,-1.17203152359781E-12,-1.));
#10834=DIRECTION('',(1.,0.,0.));
#10835=DIRECTION('center_axis',(1.,0.,0.));
#10836=DIRECTION('ref_axis',(0.,-1.17203152359781E-12,-1.));
#10837=DIRECTION('',(1.,0.,0.));
#10838=DIRECTION('center_axis',(1.,0.,0.));
#10839=DIRECTION('ref_axis',(0.,-1.17203152359781E-12,-1.));
#10840=DIRECTION('',(1.,0.,0.));
#10841=DIRECTION('center_axis',(1.,0.,0.));
#10842=DIRECTION('ref_axis',(0.,-1.17203152359781E-12,-1.));
#10843=DIRECTION('center_axis',(-1.,0.,0.));
#10844=DIRECTION('ref_axis',(0.,-1.17203152359781E-12,-1.));
#10845=DIRECTION('center_axis',(0.,1.,0.));
#10846=DIRECTION('ref_axis',(0.,0.,1.));
#10847=DIRECTION('',(-1.,0.,0.));
#10848=DIRECTION('',(0.,0.,1.));
#10849=DIRECTION('',(1.,0.,0.));
#10850=DIRECTION('',(0.,0.,1.));
#10851=DIRECTION('center_axis',(1.,0.,0.));
#10852=DIRECTION('ref_axis',(0.,0.,-1.));
#10853=DIRECTION('center_axis',(-1.,0.,0.));
#10854=DIRECTION('ref_axis',(0.,0.,-1.));
#10855=DIRECTION('',(0.,-1.,0.));
#10856=DIRECTION('',(0.,0.,-1.));
#10857=DIRECTION('center_axis',(0.,0.,1.));
#10858=DIRECTION('ref_axis',(0.,-1.,0.));
#10859=DIRECTION('',(0.,-1.,0.));
#10860=DIRECTION('',(1.,0.,0.));
#10861=DIRECTION('center_axis',(0.,-1.,0.));
#10862=DIRECTION('ref_axis',(0.,0.,-1.));
#10863=DIRECTION('',(1.,0.,0.));
#10864=DIRECTION('',(0.,0.,-1.));
#10865=DIRECTION('center_axis',(1.,0.,0.));
#10866=DIRECTION('ref_axis',(0.,0.,-1.));
#10867=DIRECTION('center_axis',(1.,0.,0.));
#10868=DIRECTION('ref_axis',(0.,0.,-1.));
#10869=DIRECTION('center_axis',(1.,0.,0.));
#10870=DIRECTION('ref_axis',(0.,0.,-1.));
#10871=DIRECTION('center_axis',(1.,0.,0.));
#10872=DIRECTION('ref_axis',(0.,0.,-1.));
#10873=DIRECTION('',(-1.,0.,0.));
#10874=DIRECTION('center_axis',(-1.,0.,0.));
#10875=DIRECTION('ref_axis',(0.,0.,-1.));
#10876=DIRECTION('center_axis',(1.,0.,0.));
#10877=DIRECTION('ref_axis',(0.,0.,-1.));
#10878=DIRECTION('center_axis',(1.,0.,0.));
#10879=DIRECTION('ref_axis',(0.,0.,-1.));
#10880=DIRECTION('center_axis',(1.,0.,0.));
#10881=DIRECTION('ref_axis',(0.,0.,-1.));
#10882=DIRECTION('center_axis',(-1.,0.,0.));
#10883=DIRECTION('ref_axis',(0.,0.,-1.));
#10884=DIRECTION('center_axis',(1.,0.,0.));
#10885=DIRECTION('ref_axis',(0.,0.,-1.));
#10886=DIRECTION('center_axis',(1.,0.,0.));
#10887=DIRECTION('ref_axis',(0.,0.,-1.));
#10888=DIRECTION('',(-1.,0.,0.));
#10889=DIRECTION('center_axis',(1.,0.,0.));
#10890=DIRECTION('ref_axis',(0.,0.,-1.));
#10891=DIRECTION('center_axis',(1.,0.,0.));
#10892=DIRECTION('ref_axis',(0.,0.,-1.));
#10893=DIRECTION('center_axis',(1.,0.,0.));
#10894=DIRECTION('ref_axis',(0.,0.,-1.));
#10895=DIRECTION('axis',(0.,0.,1.));
#10896=DIRECTION('refdir',(1.,0.,0.));
#10897=DIRECTION('center_axis',(1.,0.,0.));
#10898=DIRECTION('ref_axis',(0.,0.,-1.));
#10899=DIRECTION('center_axis',(-1.,0.,0.));
#10900=DIRECTION('ref_axis',(0.,0.,-1.));
#10901=DIRECTION('',(-1.,0.,0.));
#10902=DIRECTION('center_axis',(-1.,0.,0.));
#10903=DIRECTION('ref_axis',(0.,0.,-1.));
#10904=DIRECTION('center_axis',(1.,0.,0.));
#10905=DIRECTION('ref_axis',(0.,0.,-1.));
#10906=DIRECTION('center_axis',(1.,0.,0.));
#10907=DIRECTION('ref_axis',(0.,0.,-1.));
#10908=DIRECTION('',(-1.,0.,0.));
#10909=DIRECTION('center_axis',(1.,0.,0.));
#10910=DIRECTION('ref_axis',(0.,0.,-1.));
#10911=DIRECTION('center_axis',(1.,0.,0.));
#10912=DIRECTION('ref_axis',(0.,0.,-1.));
#10913=DIRECTION('center_axis',(1.,0.,0.));
#10914=DIRECTION('ref_axis',(0.,0.,-1.));
#10915=DIRECTION('axis',(0.,0.,1.));
#10916=DIRECTION('refdir',(1.,0.,0.));
#10917=DIRECTION('center_axis',(0.,1.,0.));
#10918=DIRECTION('ref_axis',(1.,0.,0.));
#10919=DIRECTION('',(1.,0.,0.));
#10920=DIRECTION('center_axis',(0.,1.,0.));
#10921=DIRECTION('ref_axis',(1.,0.,0.));
#10922=DIRECTION('center_axis',(0.,1.,0.));
#10923=DIRECTION('ref_axis',(1.,0.,0.));
#10924=DIRECTION('center_axis',(0.,1.,0.));
#10925=DIRECTION('ref_axis',(1.,0.,0.));
#10926=DIRECTION('',(0.,1.,0.));
#10927=DIRECTION('center_axis',(0.,1.,0.));
#10928=DIRECTION('ref_axis',(1.,0.,0.));
#10929=DIRECTION('',(-1.,0.,0.));
#10930=DIRECTION('center_axis',(1.,0.,0.));
#10931=DIRECTION('ref_axis',(0.,0.,-1.));
#10932=DIRECTION('center_axis',(-1.,0.,0.));
#10933=DIRECTION('ref_axis',(0.,0.,-1.));
#10934=DIRECTION('',(-1.,0.,0.));
#10935=DIRECTION('center_axis',(-1.,0.,0.));
#10936=DIRECTION('ref_axis',(0.,0.,-1.));
#10937=DIRECTION('center_axis',(1.,0.,0.));
#10938=DIRECTION('ref_axis',(0.,0.,-1.));
#10939=DIRECTION('center_axis',(1.,0.,0.));
#10940=DIRECTION('ref_axis',(0.,0.,-1.));
#10941=DIRECTION('',(-1.,0.,0.));
#10942=DIRECTION('center_axis',(1.,0.,0.));
#10943=DIRECTION('ref_axis',(0.,0.,-1.));
#10944=DIRECTION('center_axis',(1.,0.,0.));
#10945=DIRECTION('ref_axis',(0.,0.,-1.));
#10946=DIRECTION('center_axis',(1.,0.,0.));
#10947=DIRECTION('ref_axis',(0.,0.,-1.));
#10948=DIRECTION('axis',(0.,0.,1.));
#10949=DIRECTION('refdir',(1.,0.,0.));
#10950=DIRECTION('center_axis',(1.,0.,0.));
#10951=DIRECTION('ref_axis',(0.,0.,-1.));
#10952=DIRECTION('center_axis',(1.,0.,0.));
#10953=DIRECTION('ref_axis',(0.,0.,-1.));
#10954=DIRECTION('',(1.,0.,0.));
#10955=DIRECTION('center_axis',(-1.,0.,0.));
#10956=DIRECTION('ref_axis',(0.,0.,-1.));
#10957=DIRECTION('center_axis',(0.,1.,0.));
#10958=DIRECTION('ref_axis',(1.,0.,0.));
#10959=DIRECTION('',(1.,0.,0.));
#10960=DIRECTION('center_axis',(0.,1.,0.));
#10961=DIRECTION('ref_axis',(1.,0.,0.));
#10962=DIRECTION('center_axis',(0.,1.,0.));
#10963=DIRECTION('ref_axis',(1.,0.,0.));
#10964=DIRECTION('center_axis',(0.,1.,0.));
#10965=DIRECTION('ref_axis',(1.,0.,0.));
#10966=DIRECTION('',(0.,1.,0.));
#10967=DIRECTION('center_axis',(0.,1.,0.));
#10968=DIRECTION('ref_axis',(1.,0.,0.));
#10969=DIRECTION('',(-1.,0.,0.));
#10970=DIRECTION('center_axis',(0.,-1.,0.));
#10971=DIRECTION('ref_axis',(0.,0.,-1.));
#10972=DIRECTION('',(0.,0.,1.));
#10973=DIRECTION('',(1.,0.,0.));
#10974=DIRECTION('',(0.,0.,-1.));
#10975=DIRECTION('',(1.,0.,0.));
#10976=DIRECTION('',(0.,0.,-1.));
#10977=DIRECTION('',(-1.,0.,0.));
#10978=DIRECTION('center_axis',(0.,0.,-1.));
#10979=DIRECTION('ref_axis',(0.,1.,0.));
#10980=DIRECTION('',(0.,-1.,0.));
#10981=DIRECTION('',(1.,0.,0.));
#10982=DIRECTION('',(0.,1.,0.));
#10983=DIRECTION('center_axis',(0.,1.,0.));
#10984=DIRECTION('ref_axis',(0.,0.,1.));
#10985=DIRECTION('',(0.,0.,-1.));
#10986=DIRECTION('',(1.,0.,0.));
#10987=DIRECTION('',(0.,0.,1.));
#10988=DIRECTION('',(-1.,0.,0.));
#10989=DIRECTION('',(0.,0.,1.));
#10990=DIRECTION('center_axis',(1.,0.,0.));
#10991=DIRECTION('ref_axis',(0.,0.,-1.));
#10992=DIRECTION('center_axis',(1.,0.,0.));
#10993=DIRECTION('ref_axis',(0.,0.,-1.));
#10994=DIRECTION('center_axis',(-1.,0.,0.));
#10995=DIRECTION('ref_axis',(0.,0.,-1.));
#10996=DIRECTION('center_axis',(1.,0.,0.));
#10997=DIRECTION('ref_axis',(0.,0.,-1.));
#10998=DIRECTION('center_axis',(1.,0.,0.));
#10999=DIRECTION('ref_axis',(0.,0.,-1.));
#11000=DIRECTION('center_axis',(1.,0.,0.));
#11001=DIRECTION('ref_axis',(0.,0.,-1.));
#11002=DIRECTION('center_axis',(1.,0.,0.));
#11003=DIRECTION('ref_axis',(0.,0.,-1.));
#11004=DIRECTION('',(-1.,0.,0.));
#11005=DIRECTION('center_axis',(1.,0.,0.));
#11006=DIRECTION('ref_axis',(0.,1.22464679914735E-16,1.));
#11007=DIRECTION('center_axis',(-1.,0.,0.));
#11008=DIRECTION('ref_axis',(0.,0.,-1.));
#11009=DIRECTION('center_axis',(1.,0.,0.));
#11010=DIRECTION('ref_axis',(0.,1.22464679914735E-16,1.));
#11011=DIRECTION('center_axis',(1.,0.,0.));
#11012=DIRECTION('ref_axis',(0.,0.,-1.));
#11013=DIRECTION('center_axis',(1.,0.,0.));
#11014=DIRECTION('ref_axis',(0.,0.,-1.));
#11015=DIRECTION('axis',(0.,0.,1.));
#11016=DIRECTION('refdir',(1.,0.,0.));
#11017=DIRECTION('center_axis',(1.,0.,0.));
#11018=DIRECTION('ref_axis',(0.,0.,-1.));
#11019=DIRECTION('center_axis',(-1.,0.,0.));
#11020=DIRECTION('ref_axis',(0.,0.,-1.));
#11021=DIRECTION('',(-1.,0.,0.));
#11022=DIRECTION('center_axis',(-1.,0.,0.));
#11023=DIRECTION('ref_axis',(0.,0.,-1.));
#11024=DIRECTION('center_axis',(1.,0.,0.));
#11025=DIRECTION('ref_axis',(0.,0.,-1.));
#11026=DIRECTION('center_axis',(1.,0.,0.));
#11027=DIRECTION('ref_axis',(0.,0.,-1.));
#11028=DIRECTION('',(-1.,0.,0.));
#11029=DIRECTION('center_axis',(1.,0.,0.));
#11030=DIRECTION('ref_axis',(0.,0.,-1.));
#11031=DIRECTION('center_axis',(1.,0.,0.));
#11032=DIRECTION('ref_axis',(0.,0.,-1.));
#11033=DIRECTION('center_axis',(1.,0.,0.));
#11034=DIRECTION('ref_axis',(0.,0.,-1.));
#11035=DIRECTION('axis',(0.,0.,1.));
#11036=DIRECTION('refdir',(1.,0.,0.));
#11037=DIRECTION('center_axis',(1.,0.,0.));
#11038=DIRECTION('ref_axis',(0.,0.,-1.));
#11039=DIRECTION('center_axis',(-1.,0.,0.));
#11040=DIRECTION('ref_axis',(0.,0.,-1.));
#11041=DIRECTION('',(-1.,0.,0.));
#11042=DIRECTION('center_axis',(-1.,0.,0.));
#11043=DIRECTION('ref_axis',(0.,0.,-1.));
#11044=DIRECTION('center_axis',(1.,0.,0.));
#11045=DIRECTION('ref_axis',(0.,0.,-1.));
#11046=DIRECTION('center_axis',(1.,0.,0.));
#11047=DIRECTION('ref_axis',(0.,0.,-1.));
#11048=DIRECTION('',(-1.,0.,0.));
#11049=DIRECTION('center_axis',(1.,0.,0.));
#11050=DIRECTION('ref_axis',(0.,0.,-1.));
#11051=DIRECTION('center_axis',(1.,0.,0.));
#11052=DIRECTION('ref_axis',(0.,0.,-1.));
#11053=DIRECTION('center_axis',(1.,0.,0.));
#11054=DIRECTION('ref_axis',(0.,0.,-1.));
#11055=DIRECTION('axis',(0.,0.,1.));
#11056=DIRECTION('refdir',(1.,0.,0.));
#11057=DIRECTION('center_axis',(1.,0.,0.));
#11058=DIRECTION('ref_axis',(0.,0.,-1.));
#11059=DIRECTION('',(0.,-0.707106781186547,-0.707106781186548));
#11060=DIRECTION('',(0.,-1.,0.));
#11061=DIRECTION('',(0.,-0.707106781186547,0.707106781186548));
#11062=DIRECTION('',(0.,0.,1.));
#11063=DIRECTION('',(0.,0.707106781186547,0.707106781186548));
#11064=DIRECTION('',(0.,1.,0.));
#11065=DIRECTION('',(0.,0.707106781186547,-0.707106781186548));
#11066=DIRECTION('',(0.,0.,-1.));
#11067=DIRECTION('center_axis',(0.,0.707106781186548,-0.707106781186547));
#11068=DIRECTION('ref_axis',(-1.,0.,0.));
#11069=DIRECTION('',(1.,0.,0.));
#11070=DIRECTION('',(0.,-0.707106781186547,-0.707106781186548));
#11071=DIRECTION('',(-1.,0.,0.));
#11072=DIRECTION('center_axis',(0.,1.,0.));
#11073=DIRECTION('ref_axis',(-1.,0.,0.));
#11074=DIRECTION('',(-1.,0.,0.));
#11075=DIRECTION('',(0.,0.,-1.));
#11076=DIRECTION('center_axis',(0.,0.707106781186548,0.707106781186547));
#11077=DIRECTION('ref_axis',(1.,0.,0.));
#11078=DIRECTION('',(1.,0.,0.));
#11079=DIRECTION('',(0.,0.707106781186547,-0.707106781186548));
#11080=DIRECTION('center_axis',(0.,0.,1.));
#11081=DIRECTION('ref_axis',(1.,0.,0.));
#11082=DIRECTION('',(-1.,0.,0.));
#11083=DIRECTION('',(0.,1.,0.));
#11084=DIRECTION('center_axis',(1.,0.,0.));
#11085=DIRECTION('ref_axis',(0.,0.,-1.));
#11086=DIRECTION('',(0.,-0.707106781186547,0.707106781186548));
#11087=DIRECTION('',(0.,-1.,0.));
#11088=DIRECTION('',(0.,0.707106781186547,0.707106781186548));
#11089=DIRECTION('',(0.,0.,1.));
#11090=DIRECTION('center_axis',(0.,0.,1.));
#11091=DIRECTION('ref_axis',(1.,0.,0.));
#11092=DIRECTION('',(1.,0.,0.));
#11093=DIRECTION('center_axis',(0.,-0.707106781186548,0.707106781186547));
#11094=DIRECTION('ref_axis',(1.,0.,0.));
#11095=DIRECTION('',(1.,0.,0.));
#11096=DIRECTION('center_axis',(0.,-0.707106781186548,-0.707106781186547));
#11097=DIRECTION('ref_axis',(-1.,0.,0.));
#11098=DIRECTION('',(-1.,0.,0.));
#11099=DIRECTION('center_axis',(0.,-1.,0.));
#11100=DIRECTION('ref_axis',(1.,0.,0.));
#11101=DIRECTION('axis',(0.,0.,1.));
#11102=DIRECTION('refdir',(1.,0.,0.));
#11103=DIRECTION('center_axis',(0.866025403784439,0.,-0.5));
#11104=DIRECTION('ref_axis',(0.5,0.,0.866025403784439));
#11105=DIRECTION('',(0.5,0.,0.866025403784439));
#11106=DIRECTION('',(0.,-1.,0.));
#11107=DIRECTION('',(0.5,0.,0.866025403784439));
#11108=DIRECTION('',(0.,-1.,0.));
#11109=DIRECTION('center_axis',(1.92296268638356E-16,0.,-1.));
#11110=DIRECTION('ref_axis',(1.,0.,1.92296268638356E-16));
#11111=DIRECTION('',(1.,0.,1.92296268638356E-16));
#11112=DIRECTION('',(0.,-1.,0.));
#11113=DIRECTION('',(1.,0.,1.92296268638356E-16));
#11114=DIRECTION('center_axis',(-0.866025403784439,0.,-0.5));
#11115=DIRECTION('ref_axis',(0.5,0.,-0.866025403784439));
#11116=DIRECTION('',(0.5,0.,-0.866025403784439));
#11117=DIRECTION('',(0.,-1.,0.));
#11118=DIRECTION('',(0.5,0.,-0.866025403784438));
#11119=DIRECTION('center_axis',(-0.866025403784439,0.,0.5));
#11120=DIRECTION('ref_axis',(-0.5,0.,-0.866025403784439));
#11121=DIRECTION('',(-0.5,0.,-0.866025403784439));
#11122=DIRECTION('',(0.,-1.,0.));
#11123=DIRECTION('',(-0.5,0.,-0.866025403784439));
#11124=DIRECTION('center_axis',(-1.92296268638356E-16,0.,1.));
#11125=DIRECTION('ref_axis',(-1.,0.,-1.92296268638356E-16));
#11126=DIRECTION('',(-1.,0.,-1.92296268638356E-16));
#11127=DIRECTION('',(0.,-1.,0.));
#11128=DIRECTION('',(-1.,0.,-1.92296268638356E-16));
#11129=DIRECTION('center_axis',(0.866025403784439,0.,0.5));
#11130=DIRECTION('ref_axis',(-0.5,0.,0.866025403784439));
#11131=DIRECTION('',(-0.5,0.,0.866025403784439));
#11132=DIRECTION('',(-0.5,0.,0.866025403784439));
#11133=DIRECTION('center_axis',(0.,-1.,0.));
#11134=DIRECTION('ref_axis',(0.,0.,-1.));
#11135=DIRECTION('center_axis',(0.,1.,0.));
#11136=DIRECTION('ref_axis',(0.,0.,1.));
#11137=DIRECTION('center_axis',(0.,-1.,0.));
#11138=DIRECTION('ref_axis',(1.,0.,0.));
#11139=DIRECTION('center_axis',(0.,-1.,0.));
#11140=DIRECTION('ref_axis',(1.,0.,0.));
#11141=DIRECTION('center_axis',(0.,-1.,0.));
#11142=DIRECTION('ref_axis',(1.,0.,0.));
#11143=DIRECTION('',(0.707106781186547,0.707106781186548,8.65956056235493E-17));
#11144=DIRECTION('center_axis',(0.,-1.,0.));
#11145=DIRECTION('ref_axis',(1.,0.,0.));
#11146=DIRECTION('center_axis',(0.,1.,0.));
#11147=DIRECTION('ref_axis',(1.,0.,0.));
#11148=DIRECTION('',(0.,1.,0.));
#11149=DIRECTION('center_axis',(0.,1.,0.));
#11150=DIRECTION('ref_axis',(1.,0.,0.));
#11151=DIRECTION('center_axis',(0.,-1.,0.));
#11152=DIRECTION('ref_axis',(1.,0.,0.));
#11153=DIRECTION('',(-0.707106781186547,0.707106781186548,-8.65956056235493E-17));
#11154=DIRECTION('center_axis',(0.,-1.,0.));
#11155=DIRECTION('ref_axis',(0.,0.,-1.));
#11156=DIRECTION('axis',(0.,0.,1.));
#11157=DIRECTION('refdir',(1.,0.,0.));
#11158=DIRECTION('center_axis',(0.,1.,0.));
#11159=DIRECTION('ref_axis',(1.,0.,0.));
#11160=DIRECTION('center_axis',(0.,-1.,0.));
#11161=DIRECTION('ref_axis',(1.,0.,0.));
#11162=DIRECTION('',(0.,-1.,0.));
#11163=DIRECTION('center_axis',(0.,-1.,0.));
#11164=DIRECTION('ref_axis',(1.,0.,0.));
#11165=DIRECTION('center_axis',(0.,1.,0.));
#11166=DIRECTION('ref_axis',(1.,0.,0.));
#11167=DIRECTION('center_axis',(0.,1.,0.));
#11168=DIRECTION('ref_axis',(1.,0.,0.));
#11169=DIRECTION('',(0.,-1.,0.));
#11170=DIRECTION('center_axis',(0.,1.,0.));
#11171=DIRECTION('ref_axis',(1.,0.,0.));
#11172=DIRECTION('center_axis',(0.,1.,0.));
#11173=DIRECTION('ref_axis',(1.,0.,0.));
#11174=DIRECTION('center_axis',(0.,1.,0.));
#11175=DIRECTION('ref_axis',(1.,0.,0.));
#11176=DIRECTION('axis',(0.,0.,1.));
#11177=DIRECTION('refdir',(1.,0.,0.));
#11178=DIRECTION('center_axis',(0.,1.,0.));
#11179=DIRECTION('ref_axis',(0.,0.,1.));
#11180=DIRECTION('center_axis',(0.,-1.,0.));
#11181=DIRECTION('ref_axis',(1.,0.,0.));
#11182=DIRECTION('center_axis',(0.,-1.,0.));
#11183=DIRECTION('ref_axis',(1.,0.,0.));
#11184=DIRECTION('center_axis',(0.,-1.,0.));
#11185=DIRECTION('ref_axis',(1.,0.,0.));
#11186=DIRECTION('',(0.707106781186548,0.707106781186547,8.65956056235494E-17));
#11187=DIRECTION('center_axis',(0.,-1.,0.));
#11188=DIRECTION('ref_axis',(1.,0.,0.));
#11189=DIRECTION('center_axis',(0.,-1.,0.));
#11190=DIRECTION('ref_axis',(1.,0.,0.));
#11191=DIRECTION('',(0.,1.,0.));
#11192=DIRECTION('center_axis',(0.,1.,0.));
#11193=DIRECTION('ref_axis',(1.,0.,0.));
#11194=DIRECTION('center_axis',(0.,-1.,0.));
#11195=DIRECTION('ref_axis',(1.,0.,0.));
#11196=DIRECTION('',(-0.707106781186547,0.707106781186548,-8.65956056235493E-17));
#11197=DIRECTION('center_axis',(0.,-1.,0.));
#11198=DIRECTION('ref_axis',(0.,0.,-1.));
#11199=DIRECTION('center_axis',(0.,-1.,0.));
#11200=DIRECTION('ref_axis',(1.,0.,0.));
#11201=DIRECTION('center_axis',(0.,1.,0.));
#11202=DIRECTION('ref_axis',(1.,0.,0.));
#11203=DIRECTION('center_axis',(0.,1.,0.));
#11204=DIRECTION('ref_axis',(1.,0.,0.));
#11205=DIRECTION('',(-0.447213595499958,0.894427190999916,-5.47678698264203E-17));
#11206=DIRECTION('center_axis',(0.,-1.,0.));
#11207=DIRECTION('ref_axis',(1.,0.,0.));
#11208=DIRECTION('center_axis',(0.,1.,0.));
#11209=DIRECTION('ref_axis',(1.,0.,0.));
#11210=DIRECTION('',(0.,1.,0.));
#11211=DIRECTION('center_axis',(0.,1.,0.));
#11212=DIRECTION('ref_axis',(1.,0.,0.));
#11213=DIRECTION('center_axis',(0.,-1.,0.));
#11214=DIRECTION('ref_axis',(1.,0.,0.));
#11215=DIRECTION('',(-0.707106781186547,0.707106781186548,-8.65956056235493E-17));
#11216=DIRECTION('center_axis',(0.,-1.,0.));
#11217=DIRECTION('ref_axis',(0.,0.,-1.));
#11218=DIRECTION('center_axis',(0.866025403784439,0.,-0.5));
#11219=DIRECTION('ref_axis',(0.5,0.,0.866025403784439));
#11220=DIRECTION('',(-0.5,0.,-0.866025403784439));
#11221=DIRECTION('',(0.,-1.,0.));
#11222=DIRECTION('',(0.5,0.,0.866025403784439));
#11223=DIRECTION('',(0.,-1.,0.));
#11224=DIRECTION('center_axis',(1.92296268638356E-16,0.,-1.));
#11225=DIRECTION('ref_axis',(1.,0.,1.92296268638356E-16));
#11226=DIRECTION('',(-1.,0.,-1.92296268638356E-16));
#11227=DIRECTION('',(0.,-1.,0.));
#11228=DIRECTION('',(1.,0.,1.92296268638356E-16));
#11229=DIRECTION('center_axis',(-0.866025403784439,0.,-0.5));
#11230=DIRECTION('ref_axis',(0.5,0.,-0.866025403784439));
#11231=DIRECTION('',(-0.5,0.,0.866025403784438));
#11232=DIRECTION('',(0.,-1.,0.));
#11233=DIRECTION('',(0.5,0.,-0.866025403784438));
#11234=DIRECTION('center_axis',(-0.866025403784439,0.,0.5));
#11235=DIRECTION('ref_axis',(-0.5,0.,-0.866025403784439));
#11236=DIRECTION('',(0.5,0.,0.866025403784439));
#11237=DIRECTION('',(0.,-1.,0.));
#11238=DIRECTION('',(-0.5,0.,-0.866025403784439));
#11239=DIRECTION('center_axis',(-1.92296268638356E-16,0.,1.));
#11240=DIRECTION('ref_axis',(-1.,0.,-1.92296268638356E-16));
#11241=DIRECTION('',(1.,0.,1.92296268638356E-16));
#11242=DIRECTION('',(0.,-1.,0.));
#11243=DIRECTION('',(-1.,0.,-1.92296268638356E-16));
#11244=DIRECTION('center_axis',(0.866025403784439,0.,0.5));
#11245=DIRECTION('ref_axis',(-0.5,0.,0.866025403784439));
#11246=DIRECTION('',(0.5,0.,-0.866025403784439));
#11247=DIRECTION('',(-0.5,0.,0.866025403784439));
#11248=DIRECTION('center_axis',(0.,1.,0.));
#11249=DIRECTION('ref_axis',(1.,0.,0.));
#11250=DIRECTION('center_axis',(0.,-1.,0.));
#11251=DIRECTION('ref_axis',(0.,0.,-1.));
#11252=DIRECTION('',(0.,0.,1.));
#11253=DIRECTION('',(1.,0.,0.));
#11254=DIRECTION('',(0.,0.,1.));
#11255=DIRECTION('',(1.,0.,0.));
#11256=DIRECTION('',(0.,0.,1.));
#11257=DIRECTION('',(1.,0.,0.));
#11258=DIRECTION('',(0.,0.,1.));
#11259=DIRECTION('',(1.,0.,0.));
#11260=DIRECTION('',(0.,0.,1.));
#11261=DIRECTION('',(1.,0.,0.));
#11262=DIRECTION('',(0.,0.,1.));
#11263=DIRECTION('',(1.,0.,0.));
#11264=DIRECTION('',(0.,1.,2.22044604925031E-16));
#11265=DIRECTION('',(1.,0.,0.));
#11266=DIRECTION('',(0.,1.,2.22044604925031E-16));
#11267=DIRECTION('',(1.,0.,0.));
#11268=DIRECTION('',(0.,1.,2.22044604925031E-16));
#11269=DIRECTION('',(1.,0.,0.));
#11270=DIRECTION('',(0.,1.,2.22044604925031E-16));
#11271=DIRECTION('',(1.,0.,0.));
#11272=DIRECTION('',(0.,1.,2.22044604925031E-16));
#11273=DIRECTION('',(1.,0.,0.));
#11274=DIRECTION('',(0.,1.,2.22044604925031E-16));
#11275=DIRECTION('',(1.,0.,0.));
#11276=DIRECTION('',(0.,1.,2.22044604925031E-16));
#11277=DIRECTION('',(1.,0.,0.));
#11278=DIRECTION('',(0.,0.,1.));
#11279=DIRECTION('',(2.22044604925031E-16,-1.,0.));
#11280=DIRECTION('',(0.,0.,1.));
#11281=DIRECTION('',(2.22044604925031E-16,-1.,0.));
#11282=DIRECTION('',(0.,0.,1.));
#11283=DIRECTION('',(2.22044604925031E-16,-1.,0.));
#11284=DIRECTION('',(0.,0.,1.));
#11285=DIRECTION('',(2.22044604925031E-16,-1.,0.));
#11286=DIRECTION('',(0.,0.,1.));
#11287=DIRECTION('',(2.22044604925031E-16,-1.,0.));
#11288=DIRECTION('',(0.,0.,1.));
#11289=DIRECTION('',(2.22044604925031E-16,-1.,0.));
#11290=DIRECTION('',(0.,0.,1.));
#11291=DIRECTION('',(1.,0.,0.));
#11292=DIRECTION('',(0.,0.,1.));
#11293=DIRECTION('',(1.,0.,0.));
#11294=DIRECTION('',(0.,0.,1.));
#11295=DIRECTION('',(1.,0.,0.));
#11296=DIRECTION('',(0.,0.,1.));
#11297=DIRECTION('',(1.,0.,0.));
#11298=DIRECTION('',(0.,0.,1.));
#11299=DIRECTION('',(1.,0.,0.));
#11300=DIRECTION('',(-4.39076562192853E-17,-0.995817069332362,-0.0913693845128816));
#11301=DIRECTION('',(1.00000000000001,-3.81035812533888E-17,-6.52675908485127E-17));
#11302=DIRECTION('',(0.,0.,1.));
#11303=DIRECTION('',(1.,0.,0.));
#11304=DIRECTION('',(0.,-1.22464679914735E-16,-1.));
#11305=DIRECTION('',(1.,0.,0.));
#11306=DIRECTION('',(0.,0.,1.));
#11307=DIRECTION('',(1.,0.,0.));
#11308=DIRECTION('',(0.,0.,1.));
#11309=DIRECTION('',(2.22044604925031E-16,-1.,0.));
#11310=DIRECTION('',(0.,0.,1.));
#11311=DIRECTION('',(2.22044604925031E-16,-1.,0.));
#11312=DIRECTION('',(0.,0.,1.));
#11313=DIRECTION('',(1.,0.,0.));
#11314=DIRECTION('',(6.12323399573677E-17,-3.74939945665464E-33,1.));
#11315=DIRECTION('',(1.,4.93435669623232E-63,-6.12323399573677E-17));
#11316=DIRECTION('',(5.28803320135221E-17,-0.863601359189276,-0.504175259613637));
#11317=DIRECTION('',(0.999999999999986,6.12323399573667E-17,-5.2335592413997E-33));
#11318=CARTESIAN_POINT('',(0.,0.,0.));
#11319=CARTESIAN_POINT('',(0.,0.,0.));
#11320=CARTESIAN_POINT('',(0.,0.,0.));
#11321=CARTESIAN_POINT('Origin',(11.,0.,-0.1));
#11322=CARTESIAN_POINT('',(10.67,-4.04133443718627E-17,0.));
#11323=CARTESIAN_POINT('Origin',(11.,0.,0.));
#11324=CARTESIAN_POINT('',(10.67,4.04133443718627E-17,1.2));
#11325=CARTESIAN_POINT('',(10.67,-4.04133443718627E-17,-0.1));
#11326=CARTESIAN_POINT('Origin',(11.,0.,1.2));
#11327=CARTESIAN_POINT('Origin',(1.5,-3.5,-0.1));
#11328=CARTESIAN_POINT('',(1.17,-3.5,0.));
#11329=CARTESIAN_POINT('Origin',(1.5,-3.5,0.));
#11330=CARTESIAN_POINT('',(1.17,-3.5,1.2));
#11331=CARTESIAN_POINT('',(1.17,-3.5,-0.1));
#11332=CARTESIAN_POINT('Origin',(1.5,-3.5,1.2));
#11333=CARTESIAN_POINT('Origin',(24.,-3.5,-0.1));
#11334=CARTESIAN_POINT('',(23.67,-3.5,0.));
#11335=CARTESIAN_POINT('Origin',(24.,-3.5,0.));
#11336=CARTESIAN_POINT('',(23.67,-3.5,1.2));
#11337=CARTESIAN_POINT('',(23.67,-3.5,-0.1));
#11338=CARTESIAN_POINT('Origin',(24.,-3.5,1.2));
#11339=CARTESIAN_POINT('Origin',(1.5,3.5,-0.1));
#11340=CARTESIAN_POINT('',(1.17,3.5,0.));
#11341=CARTESIAN_POINT('Origin',(1.5,3.5,0.));
#11342=CARTESIAN_POINT('',(1.17,3.5,1.2));
#11343=CARTESIAN_POINT('',(1.17,3.5,-0.1));
#11344=CARTESIAN_POINT('Origin',(1.5,3.5,1.2));
#11345=CARTESIAN_POINT('Origin',(24.,3.5,-0.1));
#11346=CARTESIAN_POINT('',(23.67,3.5,0.));
#11347=CARTESIAN_POINT('Origin',(24.,3.5,0.));
#11348=CARTESIAN_POINT('',(23.67,3.5,1.2));
#11349=CARTESIAN_POINT('',(23.67,3.5,-0.1));
#11350=CARTESIAN_POINT('Origin',(24.,3.5,1.2));
#11351=CARTESIAN_POINT('Origin',(5.,0.,-0.1));
#11352=CARTESIAN_POINT('',(4.67,-4.04133443718627E-17,0.));
#11353=CARTESIAN_POINT('Origin',(5.,0.,0.));
#11354=CARTESIAN_POINT('',(4.67,4.04133443718627E-17,1.2));
#11355=CARTESIAN_POINT('',(4.67,-4.04133443718627E-17,-0.1));
#11356=CARTESIAN_POINT('Origin',(5.,0.,1.2));
#11357=CARTESIAN_POINT('Origin',(18.,0.,-0.1));
#11358=CARTESIAN_POINT('',(17.67,-4.04133443718624E-17,0.));
#11359=CARTESIAN_POINT('Origin',(18.,0.,0.));
#11360=CARTESIAN_POINT('',(17.67,4.04133443718624E-17,1.2));
#11361=CARTESIAN_POINT('',(17.67,-4.04133443718624E-17,-0.1));
#11362=CARTESIAN_POINT('Origin',(18.,0.,1.2));
#11363=CARTESIAN_POINT('Origin',(26.,5.5,0.));
#11364=CARTESIAN_POINT('',(26.,5.5,0.));
#11365=CARTESIAN_POINT('',(0.,5.5,0.));
#11366=CARTESIAN_POINT('',(26.,5.5,0.));
#11367=CARTESIAN_POINT('',(0.,5.5,1.2));
#11368=CARTESIAN_POINT('',(0.,5.5,0.));
#11369=CARTESIAN_POINT('',(26.,5.5,1.2));
#11370=CARTESIAN_POINT('',(26.,5.5,1.2));
#11371=CARTESIAN_POINT('',(26.,5.5,0.));
#11372=CARTESIAN_POINT('Origin',(26.,-5.5,0.));
#11373=CARTESIAN_POINT('',(26.,-5.5,0.));
#11374=CARTESIAN_POINT('',(26.,-5.5,0.));
#11375=CARTESIAN_POINT('',(26.,-5.5,1.2));
#11376=CARTESIAN_POINT('',(26.,-5.5,1.2));
#11377=CARTESIAN_POINT('',(26.,-5.5,0.));
#11378=CARTESIAN_POINT('Origin',(0.,-5.5,0.));
#11379=CARTESIAN_POINT('',(0.,-5.5,0.));
#11380=CARTESIAN_POINT('',(0.,-5.5,0.));
#11381=CARTESIAN_POINT('',(0.,-5.5,1.2));
#11382=CARTESIAN_POINT('',(0.,-5.5,1.2));
#11383=CARTESIAN_POINT('',(0.,-5.5,0.));
#11384=CARTESIAN_POINT('Origin',(0.,5.5,0.));
#11385=CARTESIAN_POINT('',(0.,5.5,0.));
#11386=CARTESIAN_POINT('',(0.,5.5,1.2));
#11387=CARTESIAN_POINT('Origin',(13.,0.,1.2));
#11388=CARTESIAN_POINT('Origin',(13.,0.,0.));
#11389=CARTESIAN_POINT('',(0.,0.,0.));
#11390=CARTESIAN_POINT('Origin',(5.,0.,1.1));
#11391=CARTESIAN_POINT('',(4.75,-3.06161699786838E-17,1.2));
#11392=CARTESIAN_POINT('Origin',(5.,0.,1.2));
#11393=CARTESIAN_POINT('',(4.75,-3.06161699786838E-17,2.1));
#11394=CARTESIAN_POINT('',(4.75,-3.06161699786838E-17,1.1));
#11395=CARTESIAN_POINT('Origin',(5.,0.,2.1));
#11396=CARTESIAN_POINT('Origin',(5.,0.,2.1));
#11397=CARTESIAN_POINT('Origin',(11.,0.,1.1));
#11398=CARTESIAN_POINT('',(10.75,-3.06161699786838E-17,1.2));
#11399=CARTESIAN_POINT('Origin',(11.,0.,1.2));
#11400=CARTESIAN_POINT('',(10.75,-3.06161699786838E-17,2.1));
#11401=CARTESIAN_POINT('',(10.75,-3.06161699786838E-17,1.1));
#11402=CARTESIAN_POINT('Origin',(11.,0.,2.1));
#11403=CARTESIAN_POINT('Origin',(11.,0.,2.1));
#11404=CARTESIAN_POINT('Origin',(18.,0.,1.1));
#11405=CARTESIAN_POINT('',(17.75,-3.06161699786838E-17,1.2));
#11406=CARTESIAN_POINT('Origin',(18.,0.,1.2));
#11407=CARTESIAN_POINT('',(17.75,-3.06161699786838E-17,2.1));
#11408=CARTESIAN_POINT('',(17.75,-3.06161699786838E-17,1.1));
#11409=CARTESIAN_POINT('Origin',(18.,0.,2.1));
#11410=CARTESIAN_POINT('Origin',(18.,0.,2.1));
#11411=CARTESIAN_POINT('Origin',(3.5,2.4,2.4));
#11412=CARTESIAN_POINT('',(3.5,2.4,2.4));
#11413=CARTESIAN_POINT('',(3.5,-2.4,2.4));
#11414=CARTESIAN_POINT('',(3.5,2.4,2.4));
#11415=CARTESIAN_POINT('',(22.,-2.4,2.4));
#11416=CARTESIAN_POINT('',(3.5,-2.4,2.4));
#11417=CARTESIAN_POINT('',(22.,2.4,2.4));
#11418=CARTESIAN_POINT('',(22.,2.4,2.4));
#11419=CARTESIAN_POINT('',(3.5,2.4,2.4));
#11420=CARTESIAN_POINT('Origin',(3.5,1.8,1.2));
#11421=CARTESIAN_POINT('',(3.5,1.8,1.2));
#11422=CARTESIAN_POINT('',(3.5,1.8,1.2));
#11423=CARTESIAN_POINT('',(22.,1.8,1.2));
#11424=CARTESIAN_POINT('',(22.,1.8,1.2));
#11425=CARTESIAN_POINT('',(3.5,1.8,1.2));
#11426=CARTESIAN_POINT('Origin',(3.5,-1.8,1.2));
#11427=CARTESIAN_POINT('',(3.5,-1.8,1.2));
#11428=CARTESIAN_POINT('',(3.5,-1.8,1.2));
#11429=CARTESIAN_POINT('',(22.,-1.8,1.2));
#11430=CARTESIAN_POINT('',(22.,-1.8,1.2));
#11431=CARTESIAN_POINT('',(3.5,-1.8,1.2));
#11432=CARTESIAN_POINT('Origin',(3.5,-2.4,2.4));
#11433=CARTESIAN_POINT('',(3.5,-2.4,2.4));
#11434=CARTESIAN_POINT('',(22.,-2.4,2.4));
#11435=CARTESIAN_POINT('Origin',(22.,0.,1.8));
#11436=CARTESIAN_POINT('Origin',(3.5,0.,1.8));
#11437=CARTESIAN_POINT('',(0.,0.,0.));
#11438=CARTESIAN_POINT('Origin',(1.,-3.,5.8));
#11439=CARTESIAN_POINT('',(1.,-3.,6.01));
#11440=CARTESIAN_POINT('Origin',(1.,-3.,5.8));
#11441=CARTESIAN_POINT('',(3.,-3.,6.01));
#11442=CARTESIAN_POINT('',(1.,-3.,6.01));
#11443=CARTESIAN_POINT('Origin',(3.,-3.,5.8));
#11444=CARTESIAN_POINT('Origin',(1.,-3.,5.8));
#11445=CARTESIAN_POINT('Origin',(1.,3.,5.8));
#11446=CARTESIAN_POINT('',(1.,3.,6.01));
#11447=CARTESIAN_POINT('Origin',(1.,3.,5.8));
#11448=CARTESIAN_POINT('',(3.,3.,6.01));
#11449=CARTESIAN_POINT('',(1.,3.,6.01));
#11450=CARTESIAN_POINT('Origin',(3.,3.,5.8));
#11451=CARTESIAN_POINT('Origin',(1.,3.,5.8));
#11452=CARTESIAN_POINT('Origin',(1.5,-3.5,1.1));
#11453=CARTESIAN_POINT('',(1.25,-3.5,1.2));
#11454=CARTESIAN_POINT('Origin',(1.5,-3.5,1.2));
#11455=CARTESIAN_POINT('',(1.25,-3.5,2.9));
#11456=CARTESIAN_POINT('',(1.25,-3.5,1.1));
#11457=CARTESIAN_POINT('Origin',(1.5,-3.5,2.9));
#11458=CARTESIAN_POINT('Origin',(1.5,-3.5,2.9));
#11459=CARTESIAN_POINT('Origin',(1.5,3.5,1.1));
#11460=CARTESIAN_POINT('',(1.25,3.5,1.2));
#11461=CARTESIAN_POINT('Origin',(1.5,3.5,1.2));
#11462=CARTESIAN_POINT('',(1.25,3.5,2.9));
#11463=CARTESIAN_POINT('',(1.25,3.5,1.1));
#11464=CARTESIAN_POINT('Origin',(1.5,3.5,2.9));
#11465=CARTESIAN_POINT('Origin',(1.5,3.5,2.9));
#11466=CARTESIAN_POINT('Origin',(3.,5.,1.2));
#11467=CARTESIAN_POINT('',(3.,5.,1.2));
#11468=CARTESIAN_POINT('',(0.,5.,1.2));
#11469=CARTESIAN_POINT('',(3.,5.,1.2));
#11470=CARTESIAN_POINT('',(0.,5.,7.));
#11471=CARTESIAN_POINT('',(0.,5.,1.2));
#11472=CARTESIAN_POINT('',(3.,5.,7.));
#11473=CARTESIAN_POINT('',(3.,5.,7.));
#11474=CARTESIAN_POINT('',(3.,5.,1.2));
#11475=CARTESIAN_POINT('Origin',(3.,-5.,1.2));
#11476=CARTESIAN_POINT('',(3.,-5.,1.2));
#11477=CARTESIAN_POINT('',(3.,-5.,1.2));
#11478=CARTESIAN_POINT('',(3.,-5.,7.));
#11479=CARTESIAN_POINT('',(3.,-5.,7.));
#11480=CARTESIAN_POINT('',(3.,-5.,1.2));
#11481=CARTESIAN_POINT('Origin',(0.,-5.,1.2));
#11482=CARTESIAN_POINT('',(0.,-5.,1.2));
#11483=CARTESIAN_POINT('',(0.,-5.,1.2));
#11484=CARTESIAN_POINT('',(0.,-5.,7.));
#11485=CARTESIAN_POINT('',(0.,-5.,7.));
#11486=CARTESIAN_POINT('',(0.,-5.,1.2));
#11487=CARTESIAN_POINT('Origin',(0.,5.,1.2));
#11488=CARTESIAN_POINT('',(0.,5.,1.2));
#11489=CARTESIAN_POINT('',(0.,5.,7.));
#11490=CARTESIAN_POINT('Origin',(1.5,0.,7.));
#11491=CARTESIAN_POINT('Origin',(1.5,0.,1.2));
#11492=CARTESIAN_POINT('',(0.,0.,0.));
#11493=CARTESIAN_POINT('Origin',(22.9,2.6,4.));
#11494=CARTESIAN_POINT('',(23.,2.6,4.165));
#11495=CARTESIAN_POINT('Origin',(23.,2.6,4.));
#11496=CARTESIAN_POINT('',(25.,2.6,4.165));
#11497=CARTESIAN_POINT('',(22.9,2.6,4.165));
#11498=CARTESIAN_POINT('Origin',(25.,2.6,4.));
#11499=CARTESIAN_POINT('Origin',(22.9,1.59204083889156E-16,6.6));
#11500=CARTESIAN_POINT('',(23.,1.38997411703225E-16,6.765));
#11501=CARTESIAN_POINT('Origin',(23.,1.59204083889156E-16,6.6));
#11502=CARTESIAN_POINT('',(25.,1.79410756075087E-16,6.765));
#11503=CARTESIAN_POINT('',(22.9,1.38997411703225E-16,6.765));
#11504=CARTESIAN_POINT('Origin',(25.,1.59204083889156E-16,6.6));
#11505=CARTESIAN_POINT('Origin',(22.9,-2.6,4.));
#11506=CARTESIAN_POINT('',(23.,-2.6,4.165));
#11507=CARTESIAN_POINT('Origin',(23.,-2.6,4.));
#11508=CARTESIAN_POINT('',(25.,-2.6,4.165));
#11509=CARTESIAN_POINT('',(22.9,-2.6,4.165));
#11510=CARTESIAN_POINT('Origin',(25.,-2.6,4.));
#11511=CARTESIAN_POINT('Origin',(23.3,0.,4.));
#11512=CARTESIAN_POINT('',(23.3,-2.87791997799628E-16,6.35));
#11513=CARTESIAN_POINT('Origin',(23.3,0.,4.));
#11514=CARTESIAN_POINT('',(25.,2.87791997799628E-16,6.35));
#11515=CARTESIAN_POINT('',(23.3,-2.87791997799628E-16,6.35));
#11516=CARTESIAN_POINT('Origin',(25.,0.,4.));
#11517=CARTESIAN_POINT('Origin',(23.3,0.,4.));
#11518=CARTESIAN_POINT('',(23.3,-2.63299061816681E-16,6.15));
#11519=CARTESIAN_POINT('Origin',(23.3,0.,4.));
#11520=CARTESIAN_POINT('Origin',(22.9,0.,4.));
#11521=CARTESIAN_POINT('',(23.,-2.63299061816681E-16,6.15));
#11522=CARTESIAN_POINT('Origin',(23.,0.,4.));
#11523=CARTESIAN_POINT('',(22.9,-2.63299061816681E-16,6.15));
#11524=CARTESIAN_POINT('Origin',(24.,-3.5,1.1));
#11525=CARTESIAN_POINT('',(23.75,-3.5,1.2));
#11526=CARTESIAN_POINT('Origin',(24.,-3.5,1.2));
#11527=CARTESIAN_POINT('',(23.75,-3.5,2.9));
#11528=CARTESIAN_POINT('',(23.75,-3.5,1.1));
#11529=CARTESIAN_POINT('Origin',(24.,-3.5,2.9));
#11530=CARTESIAN_POINT('Origin',(24.,-3.5,2.9));
#11531=CARTESIAN_POINT('Origin',(24.,3.5,1.1));
#11532=CARTESIAN_POINT('',(23.75,3.5,1.2));
#11533=CARTESIAN_POINT('Origin',(24.,3.5,1.2));
#11534=CARTESIAN_POINT('',(23.75,3.5,2.9));
#11535=CARTESIAN_POINT('',(23.75,3.5,1.1));
#11536=CARTESIAN_POINT('Origin',(24.,3.5,2.9));
#11537=CARTESIAN_POINT('Origin',(24.,3.5,2.9));
#11538=CARTESIAN_POINT('Origin',(25.,5.,1.2));
#11539=CARTESIAN_POINT('',(25.,5.,1.2));
#11540=CARTESIAN_POINT('',(23.,5.,1.2));
#11541=CARTESIAN_POINT('',(25.,5.,1.2));
#11542=CARTESIAN_POINT('',(23.,5.,7.));
#11543=CARTESIAN_POINT('',(23.,5.,1.2));
#11544=CARTESIAN_POINT('',(25.,5.,7.));
#11545=CARTESIAN_POINT('',(25.,5.,7.));
#11546=CARTESIAN_POINT('',(25.,5.,1.2));
#11547=CARTESIAN_POINT('Origin',(25.,-5.,1.2));
#11548=CARTESIAN_POINT('',(25.,-5.,1.2));
#11549=CARTESIAN_POINT('',(25.,-5.,1.2));
#11550=CARTESIAN_POINT('',(25.,-5.,7.));
#11551=CARTESIAN_POINT('',(25.,-5.,7.));
#11552=CARTESIAN_POINT('',(25.,-5.,1.2));
#11553=CARTESIAN_POINT('Origin',(23.,-5.,1.2));
#11554=CARTESIAN_POINT('',(23.,-5.,1.2));
#11555=CARTESIAN_POINT('',(23.,-5.,1.2));
#11556=CARTESIAN_POINT('',(23.,-5.,7.));
#11557=CARTESIAN_POINT('',(23.,-5.,7.));
#11558=CARTESIAN_POINT('',(23.,-5.,1.2));
#11559=CARTESIAN_POINT('Origin',(23.,5.,1.2));
#11560=CARTESIAN_POINT('',(23.,5.,1.2));
#11561=CARTESIAN_POINT('',(23.,5.,7.));
#11562=CARTESIAN_POINT('Origin',(24.,0.,7.));
#11563=CARTESIAN_POINT('Origin',(24.,0.,1.2));
#11564=CARTESIAN_POINT('',(0.,0.,0.));
#11565=CARTESIAN_POINT('Origin',(24.9,2.6,4.));
#11566=CARTESIAN_POINT('',(25.,2.6,4.225));
#11567=CARTESIAN_POINT('Origin',(25.,2.6,4.));
#11568=CARTESIAN_POINT('',(25.4,2.6,4.225));
#11569=CARTESIAN_POINT('',(24.9,2.6,4.225));
#11570=CARTESIAN_POINT('Origin',(25.4,2.6,4.));
#11571=CARTESIAN_POINT('Origin',(24.9,1.59204083889156E-16,6.6));
#11572=CARTESIAN_POINT('',(25.,1.31649530908341E-16,6.825));
#11573=CARTESIAN_POINT('Origin',(25.,1.59204083889156E-16,6.6));
#11574=CARTESIAN_POINT('',(25.4,1.86758636869971E-16,6.825));
#11575=CARTESIAN_POINT('',(24.9,1.31649530908341E-16,6.825));
#11576=CARTESIAN_POINT('Origin',(25.4,1.59204083889156E-16,6.6));
#11577=CARTESIAN_POINT('Origin',(24.9,-2.6,4.));
#11578=CARTESIAN_POINT('',(25.,-2.6,4.225));
#11579=CARTESIAN_POINT('Origin',(25.,-2.6,4.));
#11580=CARTESIAN_POINT('',(25.4,-2.6,4.225));
#11581=CARTESIAN_POINT('',(24.9,-2.6,4.225));
#11582=CARTESIAN_POINT('Origin',(25.4,-2.6,4.));
#11583=CARTESIAN_POINT('Origin',(24.9,3.5,1.22));
#11584=CARTESIAN_POINT('',(25.,-1.12765242872084,1.22));
#11585=CARTESIAN_POINT('',(25.4,-1.12765242872084,1.22));
#11586=CARTESIAN_POINT('',(25.,-1.12765242872084,1.22));
#11587=CARTESIAN_POINT('',(25.,1.12765242872084,1.22));
#11588=CARTESIAN_POINT('',(25.,1.75,1.22));
#11589=CARTESIAN_POINT('',(25.4,1.12765242872084,1.22));
#11590=CARTESIAN_POINT('',(25.,1.12765242872084,1.22));
#11591=CARTESIAN_POINT('',(25.4,1.75,1.22));
#11592=CARTESIAN_POINT('Origin',(25.,0.,4.));
#11593=CARTESIAN_POINT('Origin',(25.,0.,4.));
#11594=CARTESIAN_POINT('',(25.,-2.86567351000481E-16,6.34));
#11595=CARTESIAN_POINT('Origin',(25.,0.,4.));
#11596=CARTESIAN_POINT('Origin',(25.,0.,4.));
#11597=CARTESIAN_POINT('Origin',(25.4,0.,4.));
#11598=CARTESIAN_POINT('Origin',(24.7,0.,4.));
#11599=CARTESIAN_POINT('',(24.7,-2.86567351000481E-16,6.34));
#11600=CARTESIAN_POINT('',(24.7,-2.86567351000481E-16,6.34));
#11601=CARTESIAN_POINT('Origin',(24.7,0.,4.));
#11602=CARTESIAN_POINT('Origin',(24.7,0.,4.));
#11603=CARTESIAN_POINT('',(24.7,-2.20436423846524E-16,5.8));
#11604=CARTESIAN_POINT('Origin',(24.7,0.,4.));
#11605=CARTESIAN_POINT('Origin',(25.,0.,4.));
#11606=CARTESIAN_POINT('',(25.4,-2.20436423846524E-16,5.8));
#11607=CARTESIAN_POINT('Origin',(25.4,0.,4.));
#11608=CARTESIAN_POINT('',(25.,-2.20436423846524E-16,5.8));
#11609=CARTESIAN_POINT('Origin',(25.4,0.,4.));
#11610=CARTESIAN_POINT('',(0.,0.,0.));
#11611=CARTESIAN_POINT('Origin',(14.95,3.75,5.));
#11612=CARTESIAN_POINT('',(4.,3.75,4.6));
#11613=CARTESIAN_POINT('',(4.,3.75,7.));
#11614=CARTESIAN_POINT('',(4.,3.75,4.8));
#11615=CARTESIAN_POINT('',(3.,3.75,4.6));
#11616=CARTESIAN_POINT('',(9.225,3.75,4.6));
#11617=CARTESIAN_POINT('',(3.,3.75,7.));
#11618=CARTESIAN_POINT('',(3.,3.75,4.8));
#11619=CARTESIAN_POINT('',(9.225,3.75,7.));
#11620=CARTESIAN_POINT('Origin',(3.,5.,4.6));
#11621=CARTESIAN_POINT('',(3.,-3.75,4.6));
#11622=CARTESIAN_POINT('',(3.,5.,4.6));
#11623=CARTESIAN_POINT('',(3.,-3.75,7.));
#11624=CARTESIAN_POINT('',(3.,-3.75,4.8));
#11625=CARTESIAN_POINT('',(3.,5.,7.));
#11626=CARTESIAN_POINT('',(3.,3.,6.075));
#11627=CARTESIAN_POINT('Origin',(3.,3.,5.8));
#11628=CARTESIAN_POINT('',(3.,-3.,6.075));
#11629=CARTESIAN_POINT('Origin',(3.,-3.,5.8));
#11630=CARTESIAN_POINT('Origin',(3.5,0.,4.6));
#11631=CARTESIAN_POINT('',(4.,-3.75,4.6));
#11632=CARTESIAN_POINT('',(4.,-5.,4.6));
#11633=CARTESIAN_POINT('',(9.225,-3.75,4.6));
#11634=CARTESIAN_POINT('Origin',(14.95,-3.75,5.));
#11635=CARTESIAN_POINT('',(4.,-3.75,7.));
#11636=CARTESIAN_POINT('',(4.,-3.75,4.8));
#11637=CARTESIAN_POINT('',(9.225,-3.75,7.));
#11638=CARTESIAN_POINT('Origin',(4.,-5.,4.6));
#11639=CARTESIAN_POINT('',(4.,-5.,7.));
#11640=CARTESIAN_POINT('',(4.,3.,6.275));
#11641=CARTESIAN_POINT('Origin',(4.,3.,5.8));
#11642=CARTESIAN_POINT('',(4.,-3.,6.275));
#11643=CARTESIAN_POINT('Origin',(4.,-3.,5.8));
#11644=CARTESIAN_POINT('Origin',(3.45,-3.,5.8));
#11645=CARTESIAN_POINT('',(3.45,-3.,6.275));
#11646=CARTESIAN_POINT('Origin',(3.45,-3.,5.8));
#11647=CARTESIAN_POINT('',(3.45,-3.,6.275));
#11648=CARTESIAN_POINT('Origin',(3.45,-3.,5.8));
#11649=CARTESIAN_POINT('',(3.45,-3.,6.075));
#11650=CARTESIAN_POINT('Origin',(3.45,-3.,5.8));
#11651=CARTESIAN_POINT('Origin',(3.45,3.,5.8));
#11652=CARTESIAN_POINT('',(3.45,3.,6.275));
#11653=CARTESIAN_POINT('Origin',(3.45,3.,5.8));
#11654=CARTESIAN_POINT('',(3.45,3.,6.275));
#11655=CARTESIAN_POINT('Origin',(3.45,3.,5.8));
#11656=CARTESIAN_POINT('',(3.45,3.,6.075));
#11657=CARTESIAN_POINT('Origin',(3.45,3.,5.8));
#11658=CARTESIAN_POINT('Origin',(2.9,-3.,5.8));
#11659=CARTESIAN_POINT('',(2.9,-3.,6.075));
#11660=CARTESIAN_POINT('Origin',(2.9,3.,5.8));
#11661=CARTESIAN_POINT('',(2.9,3.,6.075));
#11662=CARTESIAN_POINT('Origin',(3.5,0.,7.));
#11663=CARTESIAN_POINT('',(0.,0.,0.));
#11664=CARTESIAN_POINT('Origin',(0.144337567297406,-0.6,-0.25));
#11665=CARTESIAN_POINT('',(0.288675134594813,-0.6,0.));
#11666=CARTESIAN_POINT('',(0.144337567297406,-0.6,-0.25));
#11667=CARTESIAN_POINT('',(0.288675134594813,-0.6,0.));
#11668=CARTESIAN_POINT('',(0.144337567297406,-0.96,-0.25));
#11669=CARTESIAN_POINT('',(0.144337567297406,-0.6,-0.25));
#11670=CARTESIAN_POINT('',(0.288675134594813,-0.96,0.));
#11671=CARTESIAN_POINT('',(0.288675134594813,-0.96,0.));
#11672=CARTESIAN_POINT('',(0.288675134594813,-0.6,0.));
#11673=CARTESIAN_POINT('Origin',(-0.144337567297406,-0.6,-0.25));
#11674=CARTESIAN_POINT('',(-0.144337567297406,-0.6,-0.25));
#11675=CARTESIAN_POINT('',(0.144337567297406,-0.6,-0.25));
#11676=CARTESIAN_POINT('',(-0.144337567297406,-0.96,-0.25));
#11677=CARTESIAN_POINT('',(-0.144337567297406,-0.6,-0.25));
#11678=CARTESIAN_POINT('',(0.144337567297406,-0.96,-0.25));
#11679=CARTESIAN_POINT('Origin',(-0.288675134594813,-0.6,-8.32667268468867E-17));
#11680=CARTESIAN_POINT('',(-0.288675134594813,-0.6,-3.53525079574969E-17));
#11681=CARTESIAN_POINT('',(-0.144337567297406,-0.6,-0.25));
#11682=CARTESIAN_POINT('',(-0.288675134594813,-0.96,-5.55111512312578E-17));
#11683=CARTESIAN_POINT('',(-0.288675134594813,-0.6,-3.53525079574969E-17));
#11684=CARTESIAN_POINT('',(-0.144337567297406,-0.96,-0.25));
#11685=CARTESIAN_POINT('Origin',(-0.144337567297407,-0.6,0.25));
#11686=CARTESIAN_POINT('',(-0.144337567297407,-0.6,0.25));
#11687=CARTESIAN_POINT('',(-0.288675134594813,-0.6,-3.53525079574969E-17));
#11688=CARTESIAN_POINT('',(-0.144337567297407,-0.96,0.25));
#11689=CARTESIAN_POINT('',(-0.144337567297407,-0.6,0.25));
#11690=CARTESIAN_POINT('',(-0.288675134594813,-0.96,-3.53525079574969E-17));
#11691=CARTESIAN_POINT('Origin',(0.144337567297406,-0.6,0.25));
#11692=CARTESIAN_POINT('',(0.144337567297406,-0.6,0.25));
#11693=CARTESIAN_POINT('',(-0.144337567297407,-0.6,0.25));
#11694=CARTESIAN_POINT('',(0.144337567297406,-0.96,0.25));
#11695=CARTESIAN_POINT('',(0.144337567297406,-0.6,0.25));
#11696=CARTESIAN_POINT('',(-0.144337567297407,-0.96,0.25));
#11697=CARTESIAN_POINT('Origin',(0.288675134594813,-0.6,0.));
#11698=CARTESIAN_POINT('',(0.144337567297406,-0.6,0.25));
#11699=CARTESIAN_POINT('',(0.144337567297406,-0.96,0.25));
#11700=CARTESIAN_POINT('Origin',(0.,-0.6,0.));
#11701=CARTESIAN_POINT('Origin',(0.,-0.96,0.));
#11702=CARTESIAN_POINT('Origin',(0.,-2.,0.));
#11703=CARTESIAN_POINT('',(-0.2942,-2.,3.60291088309151E-17));
#11704=CARTESIAN_POINT('Origin',(0.,-2.,0.));
#11705=CARTESIAN_POINT('Origin',(0.45,0.6,0.));
#11706=CARTESIAN_POINT('',(-0.45,0.6,-5.51091059616309E-17));
#11707=CARTESIAN_POINT('Origin',(0.,0.6,0.));
#11708=CARTESIAN_POINT('Origin',(0.,0.575,0.));
#11709=CARTESIAN_POINT('',(-0.5,0.55,-6.12323399573677E-17));
#11710=CARTESIAN_POINT('Origin',(0.,0.55,0.));
#11711=CARTESIAN_POINT('',(-0.475,0.575,-5.81707229594993E-17));
#11712=CARTESIAN_POINT('Origin',(0.,0.29,0.));
#11713=CARTESIAN_POINT('',(-0.5,0.0299999999999998,-6.12323399573677E-17));
#11714=CARTESIAN_POINT('Origin',(0.,0.0299999999999998,0.));
#11715=CARTESIAN_POINT('',(-0.5,0.29,-6.12323399573677E-17));
#11716=CARTESIAN_POINT('Origin',(0.,0.0150000000000001,0.));
#11717=CARTESIAN_POINT('',(-0.47,7.11236625150491E-17,-5.75583995599256E-17));
#11718=CARTESIAN_POINT('Origin',(0.,0.,0.));
#11719=CARTESIAN_POINT('',(-0.485,0.0150000000000001,-5.93953697586466E-17));
#11720=CARTESIAN_POINT('Origin',(0.32,0.,0.));
#11721=CARTESIAN_POINT('',(-0.32,-6.93889390390723E-18,-3.91886975727153E-17));
#11722=CARTESIAN_POINT('Origin',(0.,0.,0.));
#11723=CARTESIAN_POINT('Origin',(0.,-0.02,0.));
#11724=CARTESIAN_POINT('',(-0.2942,-0.0515999999999999,3.60291088309151E-17));
#11725=CARTESIAN_POINT('Origin',(0.,-0.0515999999999999,0.));
#11726=CARTESIAN_POINT('',(-0.31,-0.02,-3.7964050773568E-17));
#11727=CARTESIAN_POINT('Origin',(0.,-1.24,0.));
#11728=CARTESIAN_POINT('',(-0.2942,-1.24,-3.60291088309151E-17));
#11729=CARTESIAN_POINT('',(0.,0.,0.));
#11730=CARTESIAN_POINT('',(0.,0.,0.));
#11731=CARTESIAN_POINT('Origin',(0.,0.,0.));
#11732=CARTESIAN_POINT('',(-1.63531,-0.410863395882378,-2.00267715711366E-16));
#11733=CARTESIAN_POINT('',(-2.00267715711366E-16,-0.410863395882378,1.63531));
#11734=CARTESIAN_POINT('Origin',(0.,-0.410863395882378,0.));
#11735=CARTESIAN_POINT('Origin',(0.,-0.410863395882378,0.));
#11736=CARTESIAN_POINT('',(-2.00267715711366E-16,0.410863395882378,1.63531));
#11737=CARTESIAN_POINT('Origin',(-2.05128338857182E-16,0.,1.675));
#11738=CARTESIAN_POINT('',(-1.63531,0.410863395882378,2.00267715711366E-16));
#11739=CARTESIAN_POINT('Origin',(0.,0.410863395882378,0.));
#11740=CARTESIAN_POINT('Origin',(0.,0.410863395882378,0.));
#11741=CARTESIAN_POINT('Origin',(0.,0.,0.));
#11742=CARTESIAN_POINT('',(-1.63531,0.7,-2.00267715711366E-16));
#11743=CARTESIAN_POINT('',(-1.63531,0.,-2.00267715711366E-16));
#11744=CARTESIAN_POINT('Origin',(0.,0.7,0.));
#11745=CARTESIAN_POINT('Origin',(0.,0.,0.));
#11746=CARTESIAN_POINT('',(-1.,-0.6,-1.22464679914735E-16));
#11747=CARTESIAN_POINT('Origin',(0.,-0.6,0.));
#11748=CARTESIAN_POINT('',(-1.,0.6,-1.22464679914735E-16));
#11749=CARTESIAN_POINT('',(-1.,0.,-1.22464679914735E-16));
#11750=CARTESIAN_POINT('Origin',(0.,0.6,0.));
#11751=CARTESIAN_POINT('Origin',(0.,0.65,0.));
#11752=CARTESIAN_POINT('',(-1.1,0.7,-1.34711147906209E-16));
#11753=CARTESIAN_POINT('',(-1.05,0.65,-1.28587913910472E-16));
#11754=CARTESIAN_POINT('Origin',(0.,0.7,0.));
#11755=CARTESIAN_POINT('Origin',(1.63531,0.7,0.));
#11756=CARTESIAN_POINT('Origin',(0.,0.,0.));
#11757=CARTESIAN_POINT('',(-1.63531,-0.7,-2.00267715711366E-16));
#11758=CARTESIAN_POINT('Origin',(0.,-0.7,0.));
#11759=CARTESIAN_POINT('',(-1.63531,0.,-2.00267715711366E-16));
#11760=CARTESIAN_POINT('Origin',(1.1,-0.7,0.));
#11761=CARTESIAN_POINT('',(-1.1,-0.7,-1.34711147906209E-16));
#11762=CARTESIAN_POINT('Origin',(0.,-0.7,0.));
#11763=CARTESIAN_POINT('Origin',(0.,-0.65,0.));
#11764=CARTESIAN_POINT('',(-1.05,-0.65,-1.28587913910472E-16));
#11765=CARTESIAN_POINT('',(0.,0.,0.));
#11766=CARTESIAN_POINT('Origin',(0.,0.,0.));
#11767=CARTESIAN_POINT('',(-1.71469,0.410863395882378,-2.09988962002998E-16));
#11768=CARTESIAN_POINT('',(-2.09988962002998E-16,0.410863395882378,1.71469));
#11769=CARTESIAN_POINT('Origin',(0.,0.410863395882378,0.));
#11770=CARTESIAN_POINT('Origin',(0.,0.410863395882378,0.));
#11771=CARTESIAN_POINT('',(-2.09988962002998E-16,-0.410863395882378,1.71469));
#11772=CARTESIAN_POINT('Origin',(-2.05128338857182E-16,0.,1.675));
#11773=CARTESIAN_POINT('',(-1.71469,-0.410863395882378,2.09988962002998E-16));
#11774=CARTESIAN_POINT('Origin',(0.,-0.410863395882378,0.));
#11775=CARTESIAN_POINT('Origin',(0.,-0.410863395882378,0.));
#11776=CARTESIAN_POINT('Origin',(0.,0.,0.));
#11777=CARTESIAN_POINT('',(-1.71469,-0.7,-2.09988962002998E-16));
#11778=CARTESIAN_POINT('Origin',(0.,-0.7,0.));
#11779=CARTESIAN_POINT('',(-1.71469,0.,-2.09988962002998E-16));
#11780=CARTESIAN_POINT('Origin',(2.25,0.7,0.));
#11781=CARTESIAN_POINT('',(-2.25,0.7,-2.75545529808154E-16));
#11782=CARTESIAN_POINT('Origin',(0.,0.7,0.));
#11783=CARTESIAN_POINT('',(-1.71469,0.7,-2.09988962002998E-16));
#11784=CARTESIAN_POINT('Origin',(0.,0.7,0.));
#11785=CARTESIAN_POINT('Origin',(0.,0.65,0.));
#11786=CARTESIAN_POINT('',(-2.35,0.6,-2.87791997799628E-16));
#11787=CARTESIAN_POINT('Origin',(0.,0.6,0.));
#11788=CARTESIAN_POINT('',(-2.3,0.65,-2.81668763803891E-16));
#11789=CARTESIAN_POINT('Origin',(0.,0.,0.));
#11790=CARTESIAN_POINT('',(-2.35,-0.6,-2.87791997799628E-16));
#11791=CARTESIAN_POINT('Origin',(0.,-0.6,0.));
#11792=CARTESIAN_POINT('',(-2.35,0.,-2.87791997799628E-16));
#11793=CARTESIAN_POINT('Origin',(0.,-0.65,0.));
#11794=CARTESIAN_POINT('',(-2.25,-0.7,-2.75545529808154E-16));
#11795=CARTESIAN_POINT('Origin',(0.,-0.7,0.));
#11796=CARTESIAN_POINT('',(-2.3,-0.65,-2.81668763803891E-16));
#11797=CARTESIAN_POINT('Origin',(1.71469,-0.7,0.));
#11798=CARTESIAN_POINT('Origin',(0.,0.,0.));
#11799=CARTESIAN_POINT('',(-1.71469,0.,-2.09988962002998E-16));
#11800=CARTESIAN_POINT('',(0.,0.,0.));
#11801=CARTESIAN_POINT('Origin',(1.675,0.,0.));
#11802=CARTESIAN_POINT('',(1.675,-2.97627328869245E-33,0.3969));
#11803=CARTESIAN_POINT('',(1.675,-2.97627328869245E-33,-0.3969));
#11804=CARTESIAN_POINT('Origin',(1.675,0.,0.));
#11805=CARTESIAN_POINT('Origin',(1.18440385848747,0.,-1.18440385848747));
#11806=CARTESIAN_POINT('',(1.46505453994041,3.1867025333467E-33,-0.903753177034526));
#11807=CARTESIAN_POINT('',(0.903753177034527,-9.13924911073161E-33,-1.46505453994041));
#11808=CARTESIAN_POINT('Origin',(1.18440385848747,0.,-1.18440385848747));
#11809=CARTESIAN_POINT('Origin',(1.02564169428591E-16,0.,-1.675));
#11810=CARTESIAN_POINT('',(0.3969,-2.97627328869246E-33,-1.675));
#11811=CARTESIAN_POINT('',(-0.3969,-2.97627328869245E-33,-1.675));
#11812=CARTESIAN_POINT('Origin',(1.02564169428591E-16,0.,-1.675));
#11813=CARTESIAN_POINT('Origin',(-1.18440385848747,0.,-1.18440385848747));
#11814=CARTESIAN_POINT('',(-0.903753177034526,3.1867025333467E-33,-1.46505453994041));
#11815=CARTESIAN_POINT('',(-1.46505453994041,-9.13924911073161E-33,-0.903753177034527));
#11816=CARTESIAN_POINT('Origin',(-1.18440385848747,0.,-1.18440385848747));
#11817=CARTESIAN_POINT('Origin',(-1.675,0.,-2.05128338857182E-16));
#11818=CARTESIAN_POINT('',(-1.675,-2.97627328869246E-33,-0.3969));
#11819=CARTESIAN_POINT('',(-1.675,-2.97627328869245E-33,0.3969));
#11820=CARTESIAN_POINT('Origin',(-1.675,0.,-2.05128338857182E-16));
#11821=CARTESIAN_POINT('Origin',(-1.18440385848747,0.,1.18440385848747));
#11822=CARTESIAN_POINT('',(-1.46505453994041,6.26819044436628E-33,0.903753177034526));
#11823=CARTESIAN_POINT('',(-0.903753177034527,-1.22207370217512E-32,1.46505453994041));
#11824=CARTESIAN_POINT('Origin',(-1.18440385848747,0.,1.18440385848747));
#11825=CARTESIAN_POINT('Origin',(-3.07692508285772E-16,0.,1.675));
#11826=CARTESIAN_POINT('',(-0.3969,-2.97627328869246E-33,1.675));
#11827=CARTESIAN_POINT('',(0.396899999999999,-2.97627328869245E-33,1.675));
#11828=CARTESIAN_POINT('Origin',(-3.07692508285772E-16,0.,1.675));
#11829=CARTESIAN_POINT('Origin',(1.18440385848747,0.,1.18440385848747));
#11830=CARTESIAN_POINT('',(0.903753177034526,9.34967835538585E-33,1.46505453994041));
#11831=CARTESIAN_POINT('',(1.46505453994041,-1.53022249327708E-32,0.903753177034527));
#11832=CARTESIAN_POINT('Origin',(1.18440385848747,0.,1.18440385848747));
#11833=CARTESIAN_POINT('',(0.,0.,0.));
#11834=CARTESIAN_POINT('Origin',(1.18440385848747,0.,1.18440385848747));
#11835=CARTESIAN_POINT('',(0.846804978391753,-0.07938,1.40825612658882));
#11836=CARTESIAN_POINT('',(1.40825612658882,-0.07938,0.846804978391754));
#11837=CARTESIAN_POINT('Ctrl Pts',(0.846804978391752,-0.0793800000000001,
1.40825612658882));
#11838=CARTESIAN_POINT('Ctrl Pts',(0.854205272175554,-0.123401821157026,
1.40380622184538));
#11839=CARTESIAN_POINT('Ctrl Pts',(0.867957148219441,-0.166543350814306,
1.39550172959303));
#11840=CARTESIAN_POINT('Ctrl Pts',(0.902193646979982,-0.237231147975234,
1.3735491215176));
#11841=CARTESIAN_POINT('Ctrl Pts',(0.920778333482564,-0.266264900654909,
1.36127834356734));
#11842=CARTESIAN_POINT('Ctrl Pts',(0.962485392528369,-0.317195968905306,
1.33211611256184));
#11843=CARTESIAN_POINT('Ctrl Pts',(0.985600426557816,-0.33909093068465,
1.31521005565926));
#11844=CARTESIAN_POINT('Ctrl Pts',(1.03253285680459,-0.373586846396559,
1.27866649102984));
#11845=CARTESIAN_POINT('Ctrl Pts',(1.05871835910697,-0.388086240756494,
1.25722555095714));
#11846=CARTESIAN_POINT('Ctrl Pts',(1.11153475808518,-0.407068917407805,
1.2107812086231));
#11847=CARTESIAN_POINT('Ctrl Pts',(1.13814686046673,-0.411552957311693,
1.18575674747573));
#11848=CARTESIAN_POINT('Ctrl Pts',(1.18575674747573,-0.411552957311693,
1.13814686046673));
#11849=CARTESIAN_POINT('Ctrl Pts',(1.2107812086231,-0.407068917407805,1.11153475808518));
#11850=CARTESIAN_POINT('Ctrl Pts',(1.25722555095713,-0.388086240756494,
1.05871835910697));
#11851=CARTESIAN_POINT('Ctrl Pts',(1.27866649102984,-0.373586846396559,
1.03253285680459));
#11852=CARTESIAN_POINT('Ctrl Pts',(1.31521005565926,-0.33909093068465,0.985600426557816));
#11853=CARTESIAN_POINT('Ctrl Pts',(1.33211611256184,-0.317195968905306,
0.962485392528369));
#11854=CARTESIAN_POINT('Ctrl Pts',(1.36127834356734,-0.266264900654909,
0.920778333482565));
#11855=CARTESIAN_POINT('Ctrl Pts',(1.3735491215176,-0.237231147975234,0.902193646979983));
#11856=CARTESIAN_POINT('Ctrl Pts',(1.39550172959303,-0.166543350814306,
0.867957148219442));
#11857=CARTESIAN_POINT('Ctrl Pts',(1.40380622184538,-0.123401821157026,
0.854205272175555));
#11858=CARTESIAN_POINT('Ctrl Pts',(1.40825612658882,-0.0793800000000001,
0.846804978391753));
#11859=CARTESIAN_POINT('',(0.886256117232623,-0.07938,1.45861320581289));
#11860=CARTESIAN_POINT('Origin',(1.18440385848747,-0.07938,1.18440385848747));
#11861=CARTESIAN_POINT('',(1.45861320581289,-0.07938,0.886256117232624));
#11862=CARTESIAN_POINT('Ctrl Pts',(1.45861320581289,-0.0793800000000001,
0.886256117232623));
#11863=CARTESIAN_POINT('Ctrl Pts',(1.45630208793976,-0.101649918886749,
0.890059788636852));
#11864=CARTESIAN_POINT('Ctrl Pts',(1.45296717977858,-0.123823518623746,
0.895520212222107));
#11865=CARTESIAN_POINT('Ctrl Pts',(1.43904931717599,-0.192480977588836,
0.917859913453975));
#11866=CARTESIAN_POINT('Ctrl Pts',(1.4243271592157,-0.236152929235938,0.940896403863072));
#11867=CARTESIAN_POINT('Ctrl Pts',(1.39055359345152,-0.303141259068212,
0.990027513266106));
#11868=CARTESIAN_POINT('Ctrl Pts',(1.36743459453896,-0.335108247315849,
1.02199477007745));
#11869=CARTESIAN_POINT('Ctrl Pts',(1.32643091652006,-0.373243761060364,
1.07446535104584));
#11870=CARTESIAN_POINT('Ctrl Pts',(1.30441816675528,-0.387888272594439,
1.10126842659597));
#11871=CARTESIAN_POINT('Ctrl Pts',(1.25681160160691,-0.407041111792943,
1.15530234155453));
#11872=CARTESIAN_POINT('Ctrl Pts',(1.23119764287622,-0.411552957311693,
1.18251418313119));
#11873=CARTESIAN_POINT('Ctrl Pts',(1.18251418313119,-0.411552957311693,
1.23119764287622));
#11874=CARTESIAN_POINT('Ctrl Pts',(1.15530234155453,-0.407041111792943,
1.25681160160691));
#11875=CARTESIAN_POINT('Ctrl Pts',(1.10126842659597,-0.387888272594439,
1.30441816675528));
#11876=CARTESIAN_POINT('Ctrl Pts',(1.07446535104584,-0.373243761060364,
1.32643091652006));
#11877=CARTESIAN_POINT('Ctrl Pts',(1.02199477007745,-0.335108247315848,
1.36743459453896));
#11878=CARTESIAN_POINT('Ctrl Pts',(0.990027513266105,-0.303141259068211,
1.39055359345152));
#11879=CARTESIAN_POINT('Ctrl Pts',(0.940896403863071,-0.236152929235937,
1.42432715921571));
#11880=CARTESIAN_POINT('Ctrl Pts',(0.917859913453974,-0.192480977588835,
1.43904931717599));
#11881=CARTESIAN_POINT('Ctrl Pts',(0.895520212222106,-0.123823518623745,
1.45296717977858));
#11882=CARTESIAN_POINT('Ctrl Pts',(0.890059788636851,-0.101649918886749,
1.45630208793976));
#11883=CARTESIAN_POINT('Ctrl Pts',(0.886256117232622,-0.0793800000000001,
1.45861320581289));
#11884=CARTESIAN_POINT('Origin',(1.18440385848747,-0.07938,1.18440385848747));
#11885=CARTESIAN_POINT('Origin',(0.,-0.27783,0.));
#11886=CARTESIAN_POINT('',(0.404717578595295,-0.07938,1.65807299932179));
#11887=CARTESIAN_POINT('Origin',(0.,-0.07938,0.));
#11888=CARTESIAN_POINT('',(-0.404717578595296,-0.07938,1.65807299932179));
#11889=CARTESIAN_POINT('Ctrl Pts',(0.404717578595296,-0.0793800000000001,
1.65807299932179));
#11890=CARTESIAN_POINT('Ctrl Pts',(0.400393769631747,-0.101649918886749,
1.65912839404491));
#11891=CARTESIAN_POINT('Ctrl Pts',(0.394174530911058,-0.123823518623745,
1.66063136041479));
#11892=CARTESIAN_POINT('Ctrl Pts',(0.368536561654407,-0.192480977588835,
1.66658649961961));
#11893=CARTESIAN_POINT('Ctrl Pts',(0.341837165343982,-0.236152929235937,
1.67246562047521));
#11894=CARTESIAN_POINT('Ctrl Pts',(0.283214707341173,-0.303141259068211,
1.68332504372461));
#11895=CARTESIAN_POINT('Ctrl Pts',(0.244262842368623,-0.335108247315849,
1.68958170688653));
#11896=CARTESIAN_POINT('Ctrl Pts',(0.178166559972324,-0.373243761060364,
1.69769003172132));
#11897=CARTESIAN_POINT('Ctrl Pts',(0.143648558862931,-0.387888272594439,
1.70107730356824));
#11898=CARTESIAN_POINT('Ctrl Pts',(0.0717778861362652,-0.407041111792943,
1.70562212620408));
#11899=CARTESIAN_POINT('Ctrl Pts',(0.0344244045173309,-0.411552957311693,
1.706752));
#11900=CARTESIAN_POINT('Ctrl Pts',(-0.0344244045173315,-0.411552957311693,
1.706752));
#11901=CARTESIAN_POINT('Ctrl Pts',(-0.0717778861362658,-0.407041111792943,
1.70562212620408));
#11902=CARTESIAN_POINT('Ctrl Pts',(-0.143648558862932,-0.387888272594439,
1.70107730356824));
#11903=CARTESIAN_POINT('Ctrl Pts',(-0.178166559972325,-0.373243761060364,
1.69769003172132));
#11904=CARTESIAN_POINT('Ctrl Pts',(-0.244262842368624,-0.335108247315849,
1.68958170688653));
#11905=CARTESIAN_POINT('Ctrl Pts',(-0.283214707341173,-0.303141259068212,
1.68332504372461));
#11906=CARTESIAN_POINT('Ctrl Pts',(-0.341837165343982,-0.236152929235937,
1.67246562047521));
#11907=CARTESIAN_POINT('Ctrl Pts',(-0.368536561654408,-0.192480977588835,
1.66658649961961));
#11908=CARTESIAN_POINT('Ctrl Pts',(-0.394174530911059,-0.123823518623745,
1.66063136041479));
#11909=CARTESIAN_POINT('Ctrl Pts',(-0.400393769631748,-0.101649918886749,
1.65912839404491));
#11910=CARTESIAN_POINT('Ctrl Pts',(-0.404717578595297,-0.0793800000000001,
1.65807299932179));
#11911=CARTESIAN_POINT('',(-0.886256117232624,-0.07938,1.45861320581289));
#11912=CARTESIAN_POINT('Origin',(0.,-0.07938,0.));
#11913=CARTESIAN_POINT('',(-1.45861320581289,-0.07938,0.886256117232623));
#11914=CARTESIAN_POINT('Ctrl Pts',(-0.886256117232623,-0.0793800000000001,
1.45861320581289));
#11915=CARTESIAN_POINT('Ctrl Pts',(-0.890059788636852,-0.101649918886749,
1.45630208793976));
#11916=CARTESIAN_POINT('Ctrl Pts',(-0.895520212222106,-0.123823518623745,
1.45296717977858));
#11917=CARTESIAN_POINT('Ctrl Pts',(-0.917859913453974,-0.192480977588835,
1.43904931717599));
#11918=CARTESIAN_POINT('Ctrl Pts',(-0.940896403863071,-0.236152929235937,
1.4243271592157));
#11919=CARTESIAN_POINT('Ctrl Pts',(-0.990027513266105,-0.303141259068211,
1.39055359345152));
#11920=CARTESIAN_POINT('Ctrl Pts',(-1.02199477007745,-0.335108247315848,
1.36743459453896));
#11921=CARTESIAN_POINT('Ctrl Pts',(-1.07446535104584,-0.373243761060364,
1.32643091652006));
#11922=CARTESIAN_POINT('Ctrl Pts',(-1.10126842659597,-0.387888272594439,
1.30441816675528));
#11923=CARTESIAN_POINT('Ctrl Pts',(-1.15530234155453,-0.407041111792943,
1.25681160160691));
#11924=CARTESIAN_POINT('Ctrl Pts',(-1.18251418313119,-0.411552957311693,
1.23119764287622));
#11925=CARTESIAN_POINT('Ctrl Pts',(-1.23119764287622,-0.411552957311693,
1.18251418313119));
#11926=CARTESIAN_POINT('Ctrl Pts',(-1.25681160160691,-0.407041111792943,
1.15530234155453));
#11927=CARTESIAN_POINT('Ctrl Pts',(-1.30441816675528,-0.387888272594439,
1.10126842659597));
#11928=CARTESIAN_POINT('Ctrl Pts',(-1.32643091652006,-0.373243761060365,
1.07446535104584));
#11929=CARTESIAN_POINT('Ctrl Pts',(-1.36743459453896,-0.335108247315849,
1.02199477007745));
#11930=CARTESIAN_POINT('Ctrl Pts',(-1.39055359345152,-0.303141259068212,
0.990027513266106));
#11931=CARTESIAN_POINT('Ctrl Pts',(-1.4243271592157,-0.236152929235938,
0.940896403863071));
#11932=CARTESIAN_POINT('Ctrl Pts',(-1.43904931717599,-0.192480977588836,
0.917859913453974));
#11933=CARTESIAN_POINT('Ctrl Pts',(-1.45296717977858,-0.123823518623746,
0.895520212222106));
#11934=CARTESIAN_POINT('Ctrl Pts',(-1.45630208793976,-0.101649918886749,
0.890059788636852));
#11935=CARTESIAN_POINT('Ctrl Pts',(-1.45861320581289,-0.0793800000000001,
0.886256117232623));
#11936=CARTESIAN_POINT('',(-1.65807299932179,-0.07938,0.404717578595295));
#11937=CARTESIAN_POINT('Origin',(0.,-0.07938,0.));
#11938=CARTESIAN_POINT('',(-1.706752,-0.411552957311693,2.08591827245526E-16));
#11939=CARTESIAN_POINT('Ctrl Pts',(-1.65807299932179,-0.0793800000000001,
0.404717578595296));
#11940=CARTESIAN_POINT('Ctrl Pts',(-1.65912839404491,-0.101649918886749,
0.400393769631747));
#11941=CARTESIAN_POINT('Ctrl Pts',(-1.66063136041479,-0.123823518623745,
0.394174530911058));
#11942=CARTESIAN_POINT('Ctrl Pts',(-1.66658649961961,-0.192480977588835,
0.368536561654407));
#11943=CARTESIAN_POINT('Ctrl Pts',(-1.67246562047521,-0.236152929235937,
0.341837165343982));
#11944=CARTESIAN_POINT('Ctrl Pts',(-1.68332504372461,-0.303141259068211,
0.283214707341173));
#11945=CARTESIAN_POINT('Ctrl Pts',(-1.68958170688653,-0.335108247315848,
0.244262842368623));
#11946=CARTESIAN_POINT('Ctrl Pts',(-1.69769003172132,-0.373243761060364,
0.178166559972324));
#11947=CARTESIAN_POINT('Ctrl Pts',(-1.70107730356824,-0.387888272594439,
0.143648558862931));
#11948=CARTESIAN_POINT('Ctrl Pts',(-1.70562212620408,-0.407041111792943,
0.0717778861362656));
#11949=CARTESIAN_POINT('Ctrl Pts',(-1.706752,-0.411552957311693,0.0344244045173313));
#11950=CARTESIAN_POINT('Ctrl Pts',(-1.706752,-0.411552957311693,2.08166817117217E-16));
#11951=CARTESIAN_POINT('',(-1.706752,-0.47628,2.09016837373834E-16));
#11952=CARTESIAN_POINT('',(-1.706752,-0.27783,2.09016837373834E-16));
#11953=CARTESIAN_POINT('Origin',(0.,-0.47628,0.));
#11954=CARTESIAN_POINT('',(-1.65807299932179,-0.07938,-0.404717578595296));
#11955=CARTESIAN_POINT('Ctrl Pts',(-1.706752,-0.411552957311693,2.0122792321331E-16));
#11956=CARTESIAN_POINT('Ctrl Pts',(-1.706752,-0.411552957311693,-0.0344244045173309));
#11957=CARTESIAN_POINT('Ctrl Pts',(-1.70562212620408,-0.407041111792943,
-0.0717778861362652));
#11958=CARTESIAN_POINT('Ctrl Pts',(-1.70107730356824,-0.387888272594439,
-0.143648558862931));
#11959=CARTESIAN_POINT('Ctrl Pts',(-1.69769003172132,-0.373243761060365,
-0.178166559972324));
#11960=CARTESIAN_POINT('Ctrl Pts',(-1.68958170688653,-0.335108247315849,
-0.244262842368623));
#11961=CARTESIAN_POINT('Ctrl Pts',(-1.68332504372461,-0.303141259068212,
-0.283214707341173));
#11962=CARTESIAN_POINT('Ctrl Pts',(-1.67246562047521,-0.236152929235938,
-0.341837165343982));
#11963=CARTESIAN_POINT('Ctrl Pts',(-1.66658649961961,-0.192480977588836,
-0.368536561654407));
#11964=CARTESIAN_POINT('Ctrl Pts',(-1.66063136041479,-0.123823518623745,
-0.394174530911059));
#11965=CARTESIAN_POINT('Ctrl Pts',(-1.65912839404491,-0.101649918886749,
-0.400393769631748));
#11966=CARTESIAN_POINT('Ctrl Pts',(-1.65807299932179,-0.0793800000000001,
-0.404717578595296));
#11967=CARTESIAN_POINT('',(-1.45861320581289,-0.07938,-0.886256117232623));
#11968=CARTESIAN_POINT('Origin',(0.,-0.07938,0.));
#11969=CARTESIAN_POINT('',(-0.886256117232623,-0.07938,-1.45861320581289));
#11970=CARTESIAN_POINT('Ctrl Pts',(-1.45861320581289,-0.0793800000000001,
-0.886256117232623));
#11971=CARTESIAN_POINT('Ctrl Pts',(-1.45630208793976,-0.101649918886749,
-0.890059788636852));
#11972=CARTESIAN_POINT('Ctrl Pts',(-1.45296717977858,-0.123823518623745,
-0.895520212222106));
#11973=CARTESIAN_POINT('Ctrl Pts',(-1.43904931717599,-0.192480977588835,
-0.917859913453974));
#11974=CARTESIAN_POINT('Ctrl Pts',(-1.4243271592157,-0.236152929235937,
-0.940896403863072));
#11975=CARTESIAN_POINT('Ctrl Pts',(-1.39055359345152,-0.303141259068212,
-0.990027513266106));
#11976=CARTESIAN_POINT('Ctrl Pts',(-1.36743459453896,-0.335108247315849,
-1.02199477007745));
#11977=CARTESIAN_POINT('Ctrl Pts',(-1.32643091652006,-0.373243761060364,
-1.07446535104584));
#11978=CARTESIAN_POINT('Ctrl Pts',(-1.30441816675528,-0.387888272594439,
-1.10126842659597));
#11979=CARTESIAN_POINT('Ctrl Pts',(-1.25681160160691,-0.407041111792943,
-1.15530234155453));
#11980=CARTESIAN_POINT('Ctrl Pts',(-1.23119764287622,-0.411552957311693,
-1.18251418313119));
#11981=CARTESIAN_POINT('Ctrl Pts',(-1.18251418313119,-0.411552957311693,
-1.23119764287622));
#11982=CARTESIAN_POINT('Ctrl Pts',(-1.15530234155453,-0.407041111792943,
-1.25681160160691));
#11983=CARTESIAN_POINT('Ctrl Pts',(-1.10126842659597,-0.387888272594439,
-1.30441816675528));
#11984=CARTESIAN_POINT('Ctrl Pts',(-1.07446535104584,-0.373243761060364,
-1.32643091652006));
#11985=CARTESIAN_POINT('Ctrl Pts',(-1.02199477007745,-0.335108247315848,
-1.36743459453896));
#11986=CARTESIAN_POINT('Ctrl Pts',(-0.990027513266105,-0.303141259068211,
-1.39055359345152));
#11987=CARTESIAN_POINT('Ctrl Pts',(-0.940896403863071,-0.236152929235936,
-1.42432715921571));
#11988=CARTESIAN_POINT('Ctrl Pts',(-0.917859913453974,-0.192480977588835,
-1.43904931717599));
#11989=CARTESIAN_POINT('Ctrl Pts',(-0.895520212222106,-0.123823518623745,
-1.45296717977858));
#11990=CARTESIAN_POINT('Ctrl Pts',(-0.890059788636851,-0.101649918886749,
-1.45630208793976));
#11991=CARTESIAN_POINT('Ctrl Pts',(-0.886256117232623,-0.0793800000000001,
-1.45861320581289));
#11992=CARTESIAN_POINT('',(-0.404717578595295,-0.07938,-1.65807299932179));
#11993=CARTESIAN_POINT('Origin',(0.,-0.07938,0.));
#11994=CARTESIAN_POINT('',(0.404717578595296,-0.07938,-1.65807299932179));
#11995=CARTESIAN_POINT('Ctrl Pts',(-0.404717578595296,-0.0793800000000001,
-1.65807299932179));
#11996=CARTESIAN_POINT('Ctrl Pts',(-0.400393769631747,-0.101649918886749,
-1.65912839404491));
#11997=CARTESIAN_POINT('Ctrl Pts',(-0.394174530911058,-0.123823518623746,
-1.66063136041479));
#11998=CARTESIAN_POINT('Ctrl Pts',(-0.368536561654407,-0.192480977588836,
-1.66658649961961));
#11999=CARTESIAN_POINT('Ctrl Pts',(-0.341837165343982,-0.236152929235938,
-1.67246562047521));
#12000=CARTESIAN_POINT('Ctrl Pts',(-0.283214707341173,-0.303141259068212,
-1.68332504372461));
#12001=CARTESIAN_POINT('Ctrl Pts',(-0.244262842368623,-0.335108247315849,
-1.68958170688653));
#12002=CARTESIAN_POINT('Ctrl Pts',(-0.178166559972324,-0.373243761060364,
-1.69769003172132));
#12003=CARTESIAN_POINT('Ctrl Pts',(-0.143648558862931,-0.387888272594439,
-1.70107730356824));
#12004=CARTESIAN_POINT('Ctrl Pts',(-0.0717778861362653,-0.407041111792943,
-1.70562212620408));
#12005=CARTESIAN_POINT('Ctrl Pts',(-0.034424404517331,-0.411552957311693,
-1.706752));
#12006=CARTESIAN_POINT('Ctrl Pts',(0.0344244045173312,-0.411552957311693,
-1.706752));
#12007=CARTESIAN_POINT('Ctrl Pts',(0.0717778861362655,-0.407041111792943,
-1.70562212620408));
#12008=CARTESIAN_POINT('Ctrl Pts',(0.143648558862931,-0.387888272594439,
-1.70107730356824));
#12009=CARTESIAN_POINT('Ctrl Pts',(0.178166559972324,-0.373243761060364,
-1.69769003172132));
#12010=CARTESIAN_POINT('Ctrl Pts',(0.244262842368623,-0.335108247315849,
-1.68958170688653));
#12011=CARTESIAN_POINT('Ctrl Pts',(0.283214707341173,-0.303141259068212,
-1.68332504372461));
#12012=CARTESIAN_POINT('Ctrl Pts',(0.341837165343982,-0.236152929235937,
-1.67246562047521));
#12013=CARTESIAN_POINT('Ctrl Pts',(0.368536561654407,-0.192480977588835,
-1.66658649961961));
#12014=CARTESIAN_POINT('Ctrl Pts',(0.394174530911059,-0.123823518623745,
-1.66063136041479));
#12015=CARTESIAN_POINT('Ctrl Pts',(0.400393769631748,-0.101649918886749,
-1.65912839404491));
#12016=CARTESIAN_POINT('Ctrl Pts',(0.404717578595296,-0.0793800000000001,
-1.65807299932179));
#12017=CARTESIAN_POINT('',(0.886256117232623,-0.07938,-1.45861320581289));
#12018=CARTESIAN_POINT('Origin',(0.,-0.07938,0.));
#12019=CARTESIAN_POINT('',(1.45861320581289,-0.07938,-0.886256117232623));
#12020=CARTESIAN_POINT('Ctrl Pts',(0.886256117232623,-0.0793800000000001,
-1.45861320581289));
#12021=CARTESIAN_POINT('Ctrl Pts',(0.890059788636852,-0.101649918886749,
-1.45630208793976));
#12022=CARTESIAN_POINT('Ctrl Pts',(0.895520212222106,-0.123823518623745,
-1.45296717977858));
#12023=CARTESIAN_POINT('Ctrl Pts',(0.917859913453974,-0.192480977588835,
-1.43904931717599));
#12024=CARTESIAN_POINT('Ctrl Pts',(0.940896403863072,-0.236152929235937,
-1.4243271592157));
#12025=CARTESIAN_POINT('Ctrl Pts',(0.990027513266106,-0.303141259068211,
-1.39055359345152));
#12026=CARTESIAN_POINT('Ctrl Pts',(1.02199477007745,-0.335108247315849,
-1.36743459453896));
#12027=CARTESIAN_POINT('Ctrl Pts',(1.07446535104584,-0.373243761060364,
-1.32643091652006));
#12028=CARTESIAN_POINT('Ctrl Pts',(1.10126842659597,-0.387888272594439,
-1.30441816675528));
#12029=CARTESIAN_POINT('Ctrl Pts',(1.15530234155453,-0.407041111792943,
-1.25681160160691));
#12030=CARTESIAN_POINT('Ctrl Pts',(1.18251418313119,-0.411552957311693,
-1.23119764287622));
#12031=CARTESIAN_POINT('Ctrl Pts',(1.23119764287622,-0.411552957311693,
-1.18251418313119));
#12032=CARTESIAN_POINT('Ctrl Pts',(1.25681160160691,-0.407041111792943,
-1.15530234155453));
#12033=CARTESIAN_POINT('Ctrl Pts',(1.30441816675528,-0.387888272594439,
-1.10126842659597));
#12034=CARTESIAN_POINT('Ctrl Pts',(1.32643091652006,-0.373243761060364,
-1.07446535104584));
#12035=CARTESIAN_POINT('Ctrl Pts',(1.36743459453896,-0.335108247315849,
-1.02199477007745));
#12036=CARTESIAN_POINT('Ctrl Pts',(1.39055359345152,-0.303141259068212,
-0.990027513266105));
#12037=CARTESIAN_POINT('Ctrl Pts',(1.4243271592157,-0.236152929235937,-0.940896403863071));
#12038=CARTESIAN_POINT('Ctrl Pts',(1.43904931717599,-0.192480977588835,
-0.917859913453974));
#12039=CARTESIAN_POINT('Ctrl Pts',(1.45296717977858,-0.123823518623745,
-0.895520212222106));
#12040=CARTESIAN_POINT('Ctrl Pts',(1.45630208793976,-0.101649918886749,
-0.890059788636852));
#12041=CARTESIAN_POINT('Ctrl Pts',(1.45861320581289,-0.0793800000000001,
-0.886256117232623));
#12042=CARTESIAN_POINT('',(1.65807299932179,-0.07938,-0.404717578595296));
#12043=CARTESIAN_POINT('Origin',(0.,-0.07938,0.));
#12044=CARTESIAN_POINT('',(1.65807299932179,-0.07938,0.404717578595296));
#12045=CARTESIAN_POINT('Ctrl Pts',(1.65807299932179,-0.0793800000000001,
-0.404717578595296));
#12046=CARTESIAN_POINT('Ctrl Pts',(1.65912839404491,-0.101649918886749,
-0.400393769631747));
#12047=CARTESIAN_POINT('Ctrl Pts',(1.66063136041479,-0.123823518623745,
-0.394174530911058));
#12048=CARTESIAN_POINT('Ctrl Pts',(1.66658649961961,-0.192480977588835,
-0.368536561654407));
#12049=CARTESIAN_POINT('Ctrl Pts',(1.67246562047521,-0.236152929235937,
-0.341837165343982));
#12050=CARTESIAN_POINT('Ctrl Pts',(1.68332504372461,-0.303141259068212,
-0.283214707341173));
#12051=CARTESIAN_POINT('Ctrl Pts',(1.68958170688653,-0.335108247315849,
-0.244262842368623));
#12052=CARTESIAN_POINT('Ctrl Pts',(1.69769003172132,-0.373243761060364,
-0.178166559972324));
#12053=CARTESIAN_POINT('Ctrl Pts',(1.70107730356824,-0.387888272594439,
-0.143648558862931));
#12054=CARTESIAN_POINT('Ctrl Pts',(1.70562212620408,-0.407041111792943,
-0.0717778861362655));
#12055=CARTESIAN_POINT('Ctrl Pts',(1.706752,-0.411552957311693,-0.0344244045173312));
#12056=CARTESIAN_POINT('Ctrl Pts',(1.706752,-0.411552957311693,0.0344244045173312));
#12057=CARTESIAN_POINT('Ctrl Pts',(1.70562212620408,-0.407041111792943,
0.0717778861362655));
#12058=CARTESIAN_POINT('Ctrl Pts',(1.70107730356824,-0.387888272594439,
0.143648558862931));
#12059=CARTESIAN_POINT('Ctrl Pts',(1.69769003172132,-0.373243761060364,
0.178166559972324));
#12060=CARTESIAN_POINT('Ctrl Pts',(1.68958170688653,-0.335108247315849,
0.244262842368623));
#12061=CARTESIAN_POINT('Ctrl Pts',(1.68332504372461,-0.303141259068212,
0.283214707341173));
#12062=CARTESIAN_POINT('Ctrl Pts',(1.67246562047521,-0.236152929235937,
0.341837165343982));
#12063=CARTESIAN_POINT('Ctrl Pts',(1.66658649961961,-0.192480977588835,
0.368536561654407));
#12064=CARTESIAN_POINT('Ctrl Pts',(1.66063136041479,-0.123823518623745,
0.394174530911058));
#12065=CARTESIAN_POINT('Ctrl Pts',(1.65912839404491,-0.101649918886749,
0.400393769631747));
#12066=CARTESIAN_POINT('Ctrl Pts',(1.65807299932179,-0.0793800000000001,
0.404717578595296));
#12067=CARTESIAN_POINT('Origin',(0.,-0.07938,0.));
#12068=CARTESIAN_POINT('Origin',(0.,-0.07938,0.));
#12069=CARTESIAN_POINT('',(0.397005914195118,-0.07938,1.59456899932179));
#12070=CARTESIAN_POINT('Origin',(0.,-0.07938,0.));
#12071=CARTESIAN_POINT('Origin',(-3.33066907387547E-16,-0.07938,1.675));
#12072=CARTESIAN_POINT('Origin',(-3.33066907387547E-16,0.,1.675));
#12073=CARTESIAN_POINT('',(-0.397005914195118,-0.07938,1.59456899932179));
#12074=CARTESIAN_POINT('Ctrl Pts',(-0.397005914195119,-0.0793800000000001,
1.59456899932179));
#12075=CARTESIAN_POINT('Ctrl Pts',(-0.3886265584581,-0.123401821157026,
1.59665523941937));
#12076=CARTESIAN_POINT('Ctrl Pts',(-0.373030350867485,-0.166543350814306,
1.60050712143809));
#12077=CARTESIAN_POINT('Ctrl Pts',(-0.333298652394954,-0.237231147975234,
1.60919314384089));
#12078=CARTESIAN_POINT('Ctrl Pts',(-0.311480544243687,-0.266264900654909,
1.61365775139403));
#12079=CARTESIAN_POINT('Ctrl Pts',(-0.261368388670537,-0.317195968905306,
1.62252828437015));
#12080=CARTESIAN_POINT('Ctrl Pts',(-0.233069203882014,-0.33909093068465,
1.62691869420078));
#12081=CARTESIAN_POINT('Ctrl Pts',(-0.174042761838764,-0.373586846396559,
1.63426473152765));
#12082=CARTESIAN_POINT('Ctrl Pts',(-0.14036578147155,-0.388086240756494,
1.63761964365402));
#12083=CARTESIAN_POINT('Ctrl Pts',(-0.0701778381840615,-0.407068917407805,
1.64212536811722));
#12084=CARTESIAN_POINT('Ctrl Pts',(-0.0336652739555918,-0.411552957311693,
1.643248));
#12085=CARTESIAN_POINT('Ctrl Pts',(0.0336652739555913,-0.411552957311693,
1.643248));
#12086=CARTESIAN_POINT('Ctrl Pts',(0.070177838184061,-0.407068917407805,
1.64212536811722));
#12087=CARTESIAN_POINT('Ctrl Pts',(0.140365781471549,-0.388086240756494,
1.63761964365402));
#12088=CARTESIAN_POINT('Ctrl Pts',(0.174042761838763,-0.373586846396559,
1.63426473152765));
#12089=CARTESIAN_POINT('Ctrl Pts',(0.233069203882014,-0.33909093068465,
1.62691869420078));
#12090=CARTESIAN_POINT('Ctrl Pts',(0.261368388670536,-0.317195968905306,
1.62252828437015));
#12091=CARTESIAN_POINT('Ctrl Pts',(0.311480544243686,-0.266264900654908,
1.61365775139403));
#12092=CARTESIAN_POINT('Ctrl Pts',(0.333298652394954,-0.237231147975234,
1.60919314384089));
#12093=CARTESIAN_POINT('Ctrl Pts',(0.373030350867484,-0.166543350814306,
1.60050712143809));
#12094=CARTESIAN_POINT('Ctrl Pts',(0.388626558458099,-0.123401821157026,
1.59665523941937));
#12095=CARTESIAN_POINT('Ctrl Pts',(0.397005914195118,-0.07938,1.59456899932179));
#12096=CARTESIAN_POINT('Origin',(-3.33066907387547E-16,-0.07938,1.675));
#12097=CARTESIAN_POINT('Origin',(0.,-0.07938,0.));
#12098=CARTESIAN_POINT('',(-0.846804978391754,-0.07938,1.40825612658882));
#12099=CARTESIAN_POINT('Origin',(0.,-0.07938,0.));
#12100=CARTESIAN_POINT('Origin',(-1.18440385848747,-0.07938,1.18440385848747));
#12101=CARTESIAN_POINT('Origin',(-1.18440385848747,0.,1.18440385848747));
#12102=CARTESIAN_POINT('',(-1.40825612658882,-0.07938,0.846804978391753));
#12103=CARTESIAN_POINT('Ctrl Pts',(-1.40825612658882,-0.0793800000000001,
0.846804978391753));
#12104=CARTESIAN_POINT('Ctrl Pts',(-1.40380622184538,-0.123401821157026,
0.854205272175555));
#12105=CARTESIAN_POINT('Ctrl Pts',(-1.39550172959303,-0.166543350814306,
0.867957148219442));
#12106=CARTESIAN_POINT('Ctrl Pts',(-1.3735491215176,-0.237231147975235,
0.902193646979983));
#12107=CARTESIAN_POINT('Ctrl Pts',(-1.36127834356734,-0.266264900654909,
0.920778333482565));
#12108=CARTESIAN_POINT('Ctrl Pts',(-1.33211611256184,-0.317195968905306,
0.962485392528369));
#12109=CARTESIAN_POINT('Ctrl Pts',(-1.31521005565926,-0.339090930684651,
0.985600426557816));
#12110=CARTESIAN_POINT('Ctrl Pts',(-1.27866649102984,-0.373586846396559,
1.03253285680459));
#12111=CARTESIAN_POINT('Ctrl Pts',(-1.25722555095714,-0.388086240756494,
1.05871835910697));
#12112=CARTESIAN_POINT('Ctrl Pts',(-1.2107812086231,-0.407068917407805,
1.11153475808518));
#12113=CARTESIAN_POINT('Ctrl Pts',(-1.18575674747573,-0.411552957311693,
1.13814686046673));
#12114=CARTESIAN_POINT('Ctrl Pts',(-1.13814686046673,-0.411552957311693,
1.18575674747573));
#12115=CARTESIAN_POINT('Ctrl Pts',(-1.11153475808518,-0.407068917407805,
1.2107812086231));
#12116=CARTESIAN_POINT('Ctrl Pts',(-1.05871835910697,-0.388086240756494,
1.25722555095714));
#12117=CARTESIAN_POINT('Ctrl Pts',(-1.03253285680459,-0.373586846396559,
1.27866649102984));
#12118=CARTESIAN_POINT('Ctrl Pts',(-0.985600426557816,-0.33909093068465,
1.31521005565926));
#12119=CARTESIAN_POINT('Ctrl Pts',(-0.962485392528369,-0.317195968905306,
1.33211611256184));
#12120=CARTESIAN_POINT('Ctrl Pts',(-0.920778333482565,-0.266264900654908,
1.36127834356734));
#12121=CARTESIAN_POINT('Ctrl Pts',(-0.902193646979983,-0.237231147975234,
1.3735491215176));
#12122=CARTESIAN_POINT('Ctrl Pts',(-0.867957148219442,-0.166543350814306,
1.39550172959303));
#12123=CARTESIAN_POINT('Ctrl Pts',(-0.854205272175555,-0.123401821157026,
1.40380622184538));
#12124=CARTESIAN_POINT('Ctrl Pts',(-0.846804978391753,-0.0793800000000001,
1.40825612658882));
#12125=CARTESIAN_POINT('Origin',(-1.18440385848747,-0.07938,1.18440385848747));
#12126=CARTESIAN_POINT('Origin',(0.,-0.07938,0.));
#12127=CARTESIAN_POINT('',(-1.59456899932179,-0.07938,0.397005914195118));
#12128=CARTESIAN_POINT('Origin',(0.,-0.07938,0.));
#12129=CARTESIAN_POINT('Origin',(-1.675,-0.07938,-2.22044604925031E-16));
#12130=CARTESIAN_POINT('Origin',(-1.675,0.,-2.22044604925031E-16));
#12131=CARTESIAN_POINT('',(-1.59456899932179,-0.07938,-0.397005914195118));
#12132=CARTESIAN_POINT('',(-1.643248,-0.411552957311693,3.47540551556327E-18));
#12133=CARTESIAN_POINT('Ctrl Pts',(-1.59456899932179,-0.0793800000000001,
-0.397005914195119));
#12134=CARTESIAN_POINT('Ctrl Pts',(-1.59665523941937,-0.123401821157026,
-0.388626558458099));
#12135=CARTESIAN_POINT('Ctrl Pts',(-1.60050712143809,-0.166543350814306,
-0.373030350867485));
#12136=CARTESIAN_POINT('Ctrl Pts',(-1.60919314384089,-0.237231147975234,
-0.333298652394954));
#12137=CARTESIAN_POINT('Ctrl Pts',(-1.61365775139403,-0.266264900654909,
-0.311480544243686));
#12138=CARTESIAN_POINT('Ctrl Pts',(-1.62252828437015,-0.317195968905306,
-0.261368388670537));
#12139=CARTESIAN_POINT('Ctrl Pts',(-1.62691869420078,-0.33909093068465,
-0.233069203882014));
#12140=CARTESIAN_POINT('Ctrl Pts',(-1.63426473152765,-0.373586846396559,
-0.174042761838764));
#12141=CARTESIAN_POINT('Ctrl Pts',(-1.63761964365402,-0.388086240756494,
-0.140365781471549));
#12142=CARTESIAN_POINT('Ctrl Pts',(-1.64212536811722,-0.407068917407805,
-0.0701778381840614));
#12143=CARTESIAN_POINT('Ctrl Pts',(-1.643248,-0.411552957311693,-0.0336652739555917));
#12144=CARTESIAN_POINT('Ctrl Pts',(-1.643248,-0.411552957311693,-2.0122792321331E-16));
#12145=CARTESIAN_POINT('Origin',(-1.675,-0.07938,-2.22044604925031E-16));
#12146=CARTESIAN_POINT('Ctrl Pts',(-1.643248,-0.411552957311693,-1.94289029309402E-16));
#12147=CARTESIAN_POINT('Ctrl Pts',(-1.643248,-0.411552957311693,0.0336652739555913));
#12148=CARTESIAN_POINT('Ctrl Pts',(-1.64212536811722,-0.407068917407805,
0.0701778381840609));
#12149=CARTESIAN_POINT('Ctrl Pts',(-1.63761964365402,-0.388086240756494,
0.140365781471549));
#12150=CARTESIAN_POINT('Ctrl Pts',(-1.63426473152765,-0.373586846396559,
0.174042761838763));
#12151=CARTESIAN_POINT('Ctrl Pts',(-1.62691869420078,-0.33909093068465,
0.233069203882014));
#12152=CARTESIAN_POINT('Ctrl Pts',(-1.62252828437015,-0.317195968905306,
0.261368388670536));
#12153=CARTESIAN_POINT('Ctrl Pts',(-1.61365775139403,-0.266264900654909,
0.311480544243686));
#12154=CARTESIAN_POINT('Ctrl Pts',(-1.60919314384089,-0.237231147975235,
0.333298652394954));
#12155=CARTESIAN_POINT('Ctrl Pts',(-1.60050712143809,-0.166543350814306,
0.373030350867484));
#12156=CARTESIAN_POINT('Ctrl Pts',(-1.59665523941937,-0.123401821157026,
0.388626558458099));
#12157=CARTESIAN_POINT('Ctrl Pts',(-1.59456899932179,-0.0793800000000001,
0.397005914195118));
#12158=CARTESIAN_POINT('Origin',(0.,-0.07938,0.));
#12159=CARTESIAN_POINT('',(-1.40825612658882,-0.07938,-0.846804978391753));
#12160=CARTESIAN_POINT('Origin',(0.,-0.07938,0.));
#12161=CARTESIAN_POINT('Origin',(-1.18440385848747,-0.07938,-1.18440385848747));
#12162=CARTESIAN_POINT('Origin',(-1.18440385848747,0.,-1.18440385848747));
#12163=CARTESIAN_POINT('',(-0.846804978391753,-0.07938,-1.40825612658882));
#12164=CARTESIAN_POINT('Ctrl Pts',(-0.846804978391753,-0.0793800000000001,
-1.40825612658882));
#12165=CARTESIAN_POINT('Ctrl Pts',(-0.854205272175555,-0.123401821157026,
-1.40380622184538));
#12166=CARTESIAN_POINT('Ctrl Pts',(-0.867957148219442,-0.166543350814306,
-1.39550172959303));
#12167=CARTESIAN_POINT('Ctrl Pts',(-0.902193646979982,-0.237231147975234,
-1.3735491215176));
#12168=CARTESIAN_POINT('Ctrl Pts',(-0.920778333482564,-0.266264900654908,
-1.36127834356734));
#12169=CARTESIAN_POINT('Ctrl Pts',(-0.962485392528368,-0.317195968905306,
-1.33211611256184));
#12170=CARTESIAN_POINT('Ctrl Pts',(-0.985600426557816,-0.33909093068465,
-1.31521005565926));
#12171=CARTESIAN_POINT('Ctrl Pts',(-1.03253285680459,-0.373586846396559,
-1.27866649102984));
#12172=CARTESIAN_POINT('Ctrl Pts',(-1.05871835910697,-0.388086240756494,
-1.25722555095714));
#12173=CARTESIAN_POINT('Ctrl Pts',(-1.11153475808518,-0.407068917407805,
-1.2107812086231));
#12174=CARTESIAN_POINT('Ctrl Pts',(-1.13814686046673,-0.411552957311693,
-1.18575674747573));
#12175=CARTESIAN_POINT('Ctrl Pts',(-1.18575674747573,-0.411552957311693,
-1.13814686046673));
#12176=CARTESIAN_POINT('Ctrl Pts',(-1.2107812086231,-0.407068917407805,
-1.11153475808518));
#12177=CARTESIAN_POINT('Ctrl Pts',(-1.25722555095714,-0.388086240756494,
-1.05871835910697));
#12178=CARTESIAN_POINT('Ctrl Pts',(-1.27866649102984,-0.373586846396559,
-1.03253285680459));
#12179=CARTESIAN_POINT('Ctrl Pts',(-1.31521005565926,-0.33909093068465,
-0.985600426557816));
#12180=CARTESIAN_POINT('Ctrl Pts',(-1.33211611256184,-0.317195968905306,
-0.962485392528369));
#12181=CARTESIAN_POINT('Ctrl Pts',(-1.36127834356734,-0.266264900654909,
-0.920778333482565));
#12182=CARTESIAN_POINT('Ctrl Pts',(-1.3735491215176,-0.237231147975234,
-0.902193646979983));
#12183=CARTESIAN_POINT('Ctrl Pts',(-1.39550172959303,-0.166543350814306,
-0.867957148219442));
#12184=CARTESIAN_POINT('Ctrl Pts',(-1.40380622184538,-0.123401821157026,
-0.854205272175555));
#12185=CARTESIAN_POINT('Ctrl Pts',(-1.40825612658882,-0.07938,-0.846804978391753));
#12186=CARTESIAN_POINT('Origin',(-1.18440385848747,-0.07938,-1.18440385848747));
#12187=CARTESIAN_POINT('Origin',(0.,-0.07938,0.));
#12188=CARTESIAN_POINT('',(-0.397005914195118,-0.07938,-1.59456899932179));
#12189=CARTESIAN_POINT('Origin',(0.,-0.07938,0.));
#12190=CARTESIAN_POINT('Origin',(1.11022302462516E-16,-0.07938,-1.675));
#12191=CARTESIAN_POINT('Origin',(1.11022302462516E-16,0.,-1.675));
#12192=CARTESIAN_POINT('',(0.397005914195118,-0.07938,-1.59456899932179));
#12193=CARTESIAN_POINT('Ctrl Pts',(0.397005914195119,-0.0793800000000001,
-1.59456899932179));
#12194=CARTESIAN_POINT('Ctrl Pts',(0.388626558458099,-0.123401821157026,
-1.59665523941937));
#12195=CARTESIAN_POINT('Ctrl Pts',(0.373030350867485,-0.166543350814306,
-1.60050712143809));
#12196=CARTESIAN_POINT('Ctrl Pts',(0.333298652394954,-0.237231147975234,
-1.60919314384089));
#12197=CARTESIAN_POINT('Ctrl Pts',(0.311480544243686,-0.266264900654909,
-1.61365775139403));
#12198=CARTESIAN_POINT('Ctrl Pts',(0.261368388670537,-0.317195968905306,
-1.62252828437015));
#12199=CARTESIAN_POINT('Ctrl Pts',(0.233069203882014,-0.33909093068465,
-1.62691869420078));
#12200=CARTESIAN_POINT('Ctrl Pts',(0.174042761838763,-0.373586846396559,
-1.63426473152765));
#12201=CARTESIAN_POINT('Ctrl Pts',(0.140365781471549,-0.388086240756494,
-1.63761964365402));
#12202=CARTESIAN_POINT('Ctrl Pts',(0.0701778381840612,-0.407068917407805,
-1.64212536811722));
#12203=CARTESIAN_POINT('Ctrl Pts',(0.0336652739555916,-0.411552957311693,
-1.643248));
#12204=CARTESIAN_POINT('Ctrl Pts',(-0.0336652739555915,-0.411552957311693,
-1.643248));
#12205=CARTESIAN_POINT('Ctrl Pts',(-0.0701778381840612,-0.407068917407805,
-1.64212536811722));
#12206=CARTESIAN_POINT('Ctrl Pts',(-0.140365781471549,-0.388086240756494,
-1.63761964365402));
#12207=CARTESIAN_POINT('Ctrl Pts',(-0.174042761838764,-0.373586846396559,
-1.63426473152765));
#12208=CARTESIAN_POINT('Ctrl Pts',(-0.233069203882014,-0.33909093068465,
-1.62691869420078));
#12209=CARTESIAN_POINT('Ctrl Pts',(-0.261368388670536,-0.317195968905306,
-1.62252828437015));
#12210=CARTESIAN_POINT('Ctrl Pts',(-0.311480544243686,-0.266264900654908,
-1.61365775139403));
#12211=CARTESIAN_POINT('Ctrl Pts',(-0.333298652394954,-0.237231147975234,
-1.60919314384089));
#12212=CARTESIAN_POINT('Ctrl Pts',(-0.373030350867485,-0.166543350814306,
-1.60050712143809));
#12213=CARTESIAN_POINT('Ctrl Pts',(-0.388626558458099,-0.123401821157026,
-1.59665523941937));
#12214=CARTESIAN_POINT('Ctrl Pts',(-0.397005914195118,-0.07938,-1.59456899932179));
#12215=CARTESIAN_POINT('Origin',(1.11022302462516E-16,-0.07938,-1.675));
#12216=CARTESIAN_POINT('Origin',(0.,-0.07938,0.));
#12217=CARTESIAN_POINT('',(0.846804978391753,-0.07938,-1.40825612658882));
#12218=CARTESIAN_POINT('Origin',(0.,-0.07938,0.));
#12219=CARTESIAN_POINT('Origin',(1.18440385848747,-0.07938,-1.18440385848747));
#12220=CARTESIAN_POINT('Origin',(1.18440385848747,0.,-1.18440385848747));
#12221=CARTESIAN_POINT('',(1.40825612658882,-0.07938,-0.846804978391753));
#12222=CARTESIAN_POINT('Ctrl Pts',(1.40825612658882,-0.0793800000000001,
-0.846804978391753));
#12223=CARTESIAN_POINT('Ctrl Pts',(1.40380622184538,-0.123401821157026,
-0.854205272175555));
#12224=CARTESIAN_POINT('Ctrl Pts',(1.39550172959303,-0.166543350814306,
-0.867957148219442));
#12225=CARTESIAN_POINT('Ctrl Pts',(1.3735491215176,-0.237231147975234,-0.902193646979983));
#12226=CARTESIAN_POINT('Ctrl Pts',(1.36127834356734,-0.266264900654908,
-0.920778333482565));
#12227=CARTESIAN_POINT('Ctrl Pts',(1.33211611256184,-0.317195968905306,
-0.962485392528369));
#12228=CARTESIAN_POINT('Ctrl Pts',(1.31521005565926,-0.33909093068465,-0.985600426557816));
#12229=CARTESIAN_POINT('Ctrl Pts',(1.27866649102984,-0.373586846396559,
-1.03253285680459));
#12230=CARTESIAN_POINT('Ctrl Pts',(1.25722555095714,-0.388086240756494,
-1.05871835910697));
#12231=CARTESIAN_POINT('Ctrl Pts',(1.2107812086231,-0.407068917407805,-1.11153475808518));
#12232=CARTESIAN_POINT('Ctrl Pts',(1.18575674747573,-0.411552957311693,
-1.13814686046673));
#12233=CARTESIAN_POINT('Ctrl Pts',(1.13814686046673,-0.411552957311693,
-1.18575674747573));
#12234=CARTESIAN_POINT('Ctrl Pts',(1.11153475808518,-0.407068917407805,
-1.2107812086231));
#12235=CARTESIAN_POINT('Ctrl Pts',(1.05871835910697,-0.388086240756494,
-1.25722555095714));
#12236=CARTESIAN_POINT('Ctrl Pts',(1.03253285680459,-0.373586846396559,
-1.27866649102984));
#12237=CARTESIAN_POINT('Ctrl Pts',(0.985600426557816,-0.33909093068465,
-1.31521005565926));
#12238=CARTESIAN_POINT('Ctrl Pts',(0.962485392528369,-0.317195968905306,
-1.33211611256184));
#12239=CARTESIAN_POINT('Ctrl Pts',(0.920778333482565,-0.266264900654909,
-1.36127834356734));
#12240=CARTESIAN_POINT('Ctrl Pts',(0.902193646979983,-0.237231147975234,
-1.3735491215176));
#12241=CARTESIAN_POINT('Ctrl Pts',(0.867957148219442,-0.166543350814306,
-1.39550172959303));
#12242=CARTESIAN_POINT('Ctrl Pts',(0.854205272175555,-0.123401821157026,
-1.40380622184538));
#12243=CARTESIAN_POINT('Ctrl Pts',(0.846804978391753,-0.0793800000000001,
-1.40825612658882));
#12244=CARTESIAN_POINT('Origin',(1.18440385848747,-0.07938,-1.18440385848747));
#12245=CARTESIAN_POINT('Origin',(0.,-0.27783,0.));
#12246=CARTESIAN_POINT('',(-1.643248,-0.47628,2.01239840340529E-16));
#12247=CARTESIAN_POINT('Origin',(0.,-0.47628,0.));
#12248=CARTESIAN_POINT('',(-1.643248,-0.27783,2.01239840340529E-16));
#12249=CARTESIAN_POINT('',(1.59456899932179,-0.07938,0.397005914195118));
#12250=CARTESIAN_POINT('Origin',(0.,-0.07938,0.));
#12251=CARTESIAN_POINT('',(1.59456899932179,-0.07938,-0.397005914195118));
#12252=CARTESIAN_POINT('Ctrl Pts',(1.59456899932179,-0.0793800000000001,
0.397005914195118));
#12253=CARTESIAN_POINT('Ctrl Pts',(1.59665523941937,-0.123401821157026,
0.388626558458099));
#12254=CARTESIAN_POINT('Ctrl Pts',(1.60050712143809,-0.166543350814306,
0.373030350867485));
#12255=CARTESIAN_POINT('Ctrl Pts',(1.60919314384089,-0.237231147975234,
0.333298652394954));
#12256=CARTESIAN_POINT('Ctrl Pts',(1.61365775139403,-0.266264900654909,
0.311480544243686));
#12257=CARTESIAN_POINT('Ctrl Pts',(1.62252828437015,-0.317195968905306,
0.261368388670537));
#12258=CARTESIAN_POINT('Ctrl Pts',(1.62691869420078,-0.33909093068465,0.233069203882014));
#12259=CARTESIAN_POINT('Ctrl Pts',(1.63426473152765,-0.373586846396559,
0.174042761838764));
#12260=CARTESIAN_POINT('Ctrl Pts',(1.63761964365402,-0.388086240756494,
0.140365781471549));
#12261=CARTESIAN_POINT('Ctrl Pts',(1.64212536811722,-0.407068917407805,
0.0701778381840612));
#12262=CARTESIAN_POINT('Ctrl Pts',(1.643248,-0.411552957311693,0.0336652739555916));
#12263=CARTESIAN_POINT('Ctrl Pts',(1.643248,-0.411552957311693,-0.0336652739555916));
#12264=CARTESIAN_POINT('Ctrl Pts',(1.64212536811722,-0.407068917407805,
-0.0701778381840612));
#12265=CARTESIAN_POINT('Ctrl Pts',(1.63761964365402,-0.388086240756494,
-0.140365781471549));
#12266=CARTESIAN_POINT('Ctrl Pts',(1.63426473152765,-0.373586846396559,
-0.174042761838764));
#12267=CARTESIAN_POINT('Ctrl Pts',(1.62691869420078,-0.33909093068465,-0.233069203882014));
#12268=CARTESIAN_POINT('Ctrl Pts',(1.62252828437015,-0.317195968905306,
-0.261368388670537));
#12269=CARTESIAN_POINT('Ctrl Pts',(1.61365775139403,-0.266264900654909,
-0.311480544243686));
#12270=CARTESIAN_POINT('Ctrl Pts',(1.60919314384089,-0.237231147975234,
-0.333298652394954));
#12271=CARTESIAN_POINT('Ctrl Pts',(1.60050712143809,-0.166543350814306,
-0.373030350867485));
#12272=CARTESIAN_POINT('Ctrl Pts',(1.59665523941937,-0.123401821157026,
-0.388626558458099));
#12273=CARTESIAN_POINT('Ctrl Pts',(1.59456899932179,-0.07938,-0.397005914195118));
#12274=CARTESIAN_POINT('Origin',(0.,-0.07938,0.));
#12275=CARTESIAN_POINT('Origin',(0.,-0.07938,0.));
#12276=CARTESIAN_POINT('Origin',(1.675,-0.07938,0.));
#12277=CARTESIAN_POINT('Origin',(1.675,0.,0.));
#12278=CARTESIAN_POINT('Origin',(1.675,-0.07938,0.));
#12279=CARTESIAN_POINT('Origin',(0.,-0.47628,0.));
#12280=CARTESIAN_POINT('Origin',(0.,-0.07938,0.));
#12281=CARTESIAN_POINT('',(0.,0.,0.));
#12282=CARTESIAN_POINT('Origin',(1.70469,0.695,0.));
#12283=CARTESIAN_POINT('',(-1.70469,0.695,-2.0876431520385E-16));
#12284=CARTESIAN_POINT('Origin',(0.,0.695,0.));
#12285=CARTESIAN_POINT('',(-1.65031,0.695,-2.02104685910087E-16));
#12286=CARTESIAN_POINT('Origin',(0.,0.695,0.));
#12287=CARTESIAN_POINT('Origin',(0.,0.6575,0.));
#12288=CARTESIAN_POINT('',(-1.70469,0.62,-2.0876431520385E-16));
#12289=CARTESIAN_POINT('Origin',(0.,0.62,0.));
#12290=CARTESIAN_POINT('',(-1.70469,0.6575,-2.0876431520385E-16));
#12291=CARTESIAN_POINT('Origin',(1.65031,0.62,0.));
#12292=CARTESIAN_POINT('',(-1.65031,0.62,-2.02104685910087E-16));
#12293=CARTESIAN_POINT('Origin',(0.,0.62,0.));
#12294=CARTESIAN_POINT('Origin',(0.,0.6575,0.));
#12295=CARTESIAN_POINT('',(-1.65031,0.6575,-2.02104685910087E-16));
#12296=CARTESIAN_POINT('Origin',(1.70469,-0.62,0.));
#12297=CARTESIAN_POINT('',(-1.70469,-0.62,-2.0876431520385E-16));
#12298=CARTESIAN_POINT('Origin',(0.,-0.62,0.));
#12299=CARTESIAN_POINT('',(-1.65031,-0.62,-2.02104685910087E-16));
#12300=CARTESIAN_POINT('Origin',(0.,-0.62,0.));
#12301=CARTESIAN_POINT('Origin',(0.,-0.6575,0.));
#12302=CARTESIAN_POINT('',(-1.70469,-0.695,-2.0876431520385E-16));
#12303=CARTESIAN_POINT('Origin',(0.,-0.695,0.));
#12304=CARTESIAN_POINT('',(-1.70469,-0.6575,-2.0876431520385E-16));
#12305=CARTESIAN_POINT('Origin',(1.65031,-0.695,0.));
#12306=CARTESIAN_POINT('',(-1.65031,-0.695,-2.02104685910087E-16));
#12307=CARTESIAN_POINT('Origin',(0.,-0.695,0.));
#12308=CARTESIAN_POINT('Origin',(0.,-0.6575,0.));
#12309=CARTESIAN_POINT('',(-1.65031,-0.6575,-2.02104685910087E-16));
#12310=CARTESIAN_POINT('',(0.,0.,0.));
#12311=CARTESIAN_POINT('',(0.,0.,0.));
#12312=CARTESIAN_POINT('',(0.,0.,0.));
#12313=CARTESIAN_POINT('',(0.,0.,0.));
#12314=CARTESIAN_POINT('',(0.,0.,0.));
#12315=CARTESIAN_POINT('',(0.,0.,0.));
#12316=CARTESIAN_POINT('',(0.,0.,0.));
#12317=CARTESIAN_POINT('Origin',(13.,-1.5,4.));
#12318=CARTESIAN_POINT('',(13.,-1.5,4.165));
#12319=CARTESIAN_POINT('Origin',(13.,-1.5,4.));
#12320=CARTESIAN_POINT('',(14.5,-1.5,4.165));
#12321=CARTESIAN_POINT('',(13.,-1.5,4.165));
#12322=CARTESIAN_POINT('Origin',(14.5,-1.5,4.));
#12323=CARTESIAN_POINT('Origin',(13.,-1.5,4.));
#12324=CARTESIAN_POINT('Origin',(13.,1.5,4.));
#12325=CARTESIAN_POINT('',(13.,1.5,4.165));
#12326=CARTESIAN_POINT('Origin',(13.,1.5,4.));
#12327=CARTESIAN_POINT('',(14.5,1.5,4.165));
#12328=CARTESIAN_POINT('',(13.,1.5,4.165));
#12329=CARTESIAN_POINT('Origin',(14.5,1.5,4.));
#12330=CARTESIAN_POINT('Origin',(13.,1.5,4.));
#12331=CARTESIAN_POINT('Origin',(13.,0.,5.5));
#12332=CARTESIAN_POINT('',(13.,-2.02066721859313E-17,5.665));
#12333=CARTESIAN_POINT('Origin',(13.,0.,5.5));
#12334=CARTESIAN_POINT('',(14.5,2.02066721859313E-17,5.665));
#12335=CARTESIAN_POINT('',(13.,-2.02066721859313E-17,5.665));
#12336=CARTESIAN_POINT('Origin',(14.5,0.,5.5));
#12337=CARTESIAN_POINT('Origin',(13.,0.,5.5));
#12338=CARTESIAN_POINT('Origin',(10.9,-3.,5.8));
#12339=CARTESIAN_POINT('',(11.,-3.,6.01));
#12340=CARTESIAN_POINT('Origin',(11.,-3.,5.8));
#12341=CARTESIAN_POINT('',(13.1,-3.,6.01));
#12342=CARTESIAN_POINT('',(10.9,-3.,6.01));
#12343=CARTESIAN_POINT('Origin',(13.1,-3.,5.8));
#12344=CARTESIAN_POINT('Origin',(13.1,-3.,5.8));
#12345=CARTESIAN_POINT('Origin',(10.9,3.,5.8));
#12346=CARTESIAN_POINT('',(11.,3.,6.01));
#12347=CARTESIAN_POINT('Origin',(11.,3.,5.8));
#12348=CARTESIAN_POINT('',(13.1,3.,6.01));
#12349=CARTESIAN_POINT('',(10.9,3.,6.01));
#12350=CARTESIAN_POINT('Origin',(13.1,3.,5.8));
#12351=CARTESIAN_POINT('Origin',(13.1,3.,5.8));
#12352=CARTESIAN_POINT('Origin',(13.7,4.7,2.));
#12353=CARTESIAN_POINT('',(13.225,4.7,2.));
#12354=CARTESIAN_POINT('Origin',(13.7,4.7,2.));
#12355=CARTESIAN_POINT('',(13.225,5.,2.));
#12356=CARTESIAN_POINT('',(13.225,4.7,2.));
#12357=CARTESIAN_POINT('Origin',(13.7,5.,2.));
#12358=CARTESIAN_POINT('Origin',(13.7,4.7,2.));
#12359=CARTESIAN_POINT('',(13.49,4.7,2.));
#12360=CARTESIAN_POINT('Origin',(13.7,4.7,2.));
#12361=CARTESIAN_POINT('Origin',(13.7,2.72,2.));
#12362=CARTESIAN_POINT('',(13.49,2.72,2.));
#12363=CARTESIAN_POINT('Origin',(13.7,2.72,2.));
#12364=CARTESIAN_POINT('',(13.49,2.72,2.));
#12365=CARTESIAN_POINT('Origin',(11.8,4.7,2.));
#12366=CARTESIAN_POINT('',(11.325,4.7,2.));
#12367=CARTESIAN_POINT('Origin',(11.8,4.7,2.));
#12368=CARTESIAN_POINT('',(11.325,5.,2.));
#12369=CARTESIAN_POINT('',(11.325,4.7,2.));
#12370=CARTESIAN_POINT('Origin',(11.8,5.,2.));
#12371=CARTESIAN_POINT('Origin',(11.8,4.7,2.));
#12372=CARTESIAN_POINT('',(11.59,4.7,2.));
#12373=CARTESIAN_POINT('Origin',(11.8,4.7,2.));
#12374=CARTESIAN_POINT('Origin',(11.8,2.72,2.));
#12375=CARTESIAN_POINT('',(11.59,2.72,2.));
#12376=CARTESIAN_POINT('Origin',(11.8,2.72,2.));
#12377=CARTESIAN_POINT('',(11.59,2.72,2.));
#12378=CARTESIAN_POINT('Origin',(10.9,0.,4.));
#12379=CARTESIAN_POINT('',(11.,-1.35935794705356E-16,5.11));
#12380=CARTESIAN_POINT('Origin',(11.,0.,4.));
#12381=CARTESIAN_POINT('',(14.5,1.35935794705356E-16,5.11));
#12382=CARTESIAN_POINT('',(10.9,-1.35935794705356E-16,5.11));
#12383=CARTESIAN_POINT('Origin',(14.5,0.,4.));
#12384=CARTESIAN_POINT('Origin',(10.9,2.72,1.));
#12385=CARTESIAN_POINT('',(14.5,2.72,2.42));
#12386=CARTESIAN_POINT('',(14.5,2.72,1.2));
#12387=CARTESIAN_POINT('',(14.5,2.72,1.1));
#12388=CARTESIAN_POINT('',(11.,2.72,2.42));
#12389=CARTESIAN_POINT('',(10.9,2.72,2.42));
#12390=CARTESIAN_POINT('',(11.,2.72,1.2));
#12391=CARTESIAN_POINT('',(11.,2.72,1.1));
#12392=CARTESIAN_POINT('',(11.825,2.72,1.2));
#12393=CARTESIAN_POINT('Origin',(10.9,2.72,2.42));
#12394=CARTESIAN_POINT('',(14.5,-2.42,2.42));
#12395=CARTESIAN_POINT('',(14.5,-1.14,2.42));
#12396=CARTESIAN_POINT('',(11.,-2.42,2.42));
#12397=CARTESIAN_POINT('',(10.9,-2.42,2.42));
#12398=CARTESIAN_POINT('',(11.,3.86,2.42));
#12399=CARTESIAN_POINT('Origin',(10.9,-2.42,2.42));
#12400=CARTESIAN_POINT('',(14.5,-1.90450704225352,1.2));
#12401=CARTESIAN_POINT('',(14.5,-2.39672109072547,2.36490658138361));
#12402=CARTESIAN_POINT('',(11.,-1.90450704225352,1.2));
#12403=CARTESIAN_POINT('',(11.825,-1.90450704225352,1.2));
#12404=CARTESIAN_POINT('',(11.,-1.6392728496886,0.572279077596364));
#12405=CARTESIAN_POINT('Origin',(14.5,-5.,1.2));
#12406=CARTESIAN_POINT('',(14.5,5.,1.2));
#12407=CARTESIAN_POINT('',(14.5,-5.,1.2));
#12408=CARTESIAN_POINT('',(14.5,5.,7.));
#12409=CARTESIAN_POINT('',(14.5,5.,1.2));
#12410=CARTESIAN_POINT('',(14.5,-5.,7.));
#12411=CARTESIAN_POINT('',(14.5,-5.,7.));
#12412=CARTESIAN_POINT('',(14.5,-5.,1.2));
#12413=CARTESIAN_POINT('',(14.5,-5.,1.2));
#12414=CARTESIAN_POINT('',(14.5,-5.,1.2));
#12415=CARTESIAN_POINT('Origin',(12.75,0.,1.2));
#12416=CARTESIAN_POINT('',(11.,5.,1.2));
#12417=CARTESIAN_POINT('',(11.,5.,1.2));
#12418=CARTESIAN_POINT('',(14.5,5.,1.2));
#12419=CARTESIAN_POINT('Origin',(14.5,5.,1.2));
#12420=CARTESIAN_POINT('',(11.,5.,7.));
#12421=CARTESIAN_POINT('',(11.,5.,1.2));
#12422=CARTESIAN_POINT('',(14.5,5.,7.));
#12423=CARTESIAN_POINT('Origin',(11.,-5.,1.2));
#12424=CARTESIAN_POINT('',(11.,-5.,1.2));
#12425=CARTESIAN_POINT('',(11.,-5.,1.2));
#12426=CARTESIAN_POINT('',(11.,-5.,7.));
#12427=CARTESIAN_POINT('',(11.,-5.,7.));
#12428=CARTESIAN_POINT('',(11.,-5.,1.2));
#12429=CARTESIAN_POINT('Origin',(11.,5.,1.2));
#12430=CARTESIAN_POINT('',(11.,5.,1.2));
#12431=CARTESIAN_POINT('',(11.,5.,7.));
#12432=CARTESIAN_POINT('Origin',(12.75,0.,7.));
#12433=CARTESIAN_POINT('Origin',(12.75,0.,1.2));
#12434=CARTESIAN_POINT('',(0.,0.,0.));
#12435=CARTESIAN_POINT('Origin',(11.,2.7,2.4));
#12436=CARTESIAN_POINT('',(11.,2.7,2.4));
#12437=CARTESIAN_POINT('',(11.,2.42,2.4));
#12438=CARTESIAN_POINT('',(11.,2.7,2.4));
#12439=CARTESIAN_POINT('',(14.5,2.42,2.4));
#12440=CARTESIAN_POINT('',(11.,2.42,2.4));
#12441=CARTESIAN_POINT('',(14.5,2.7,2.4));
#12442=CARTESIAN_POINT('',(14.5,2.7,2.4));
#12443=CARTESIAN_POINT('',(11.,2.7,2.4));
#12444=CARTESIAN_POINT('Origin',(11.,2.7,1.22));
#12445=CARTESIAN_POINT('',(11.,2.7,1.22));
#12446=CARTESIAN_POINT('',(11.,2.7,1.22));
#12447=CARTESIAN_POINT('',(14.5,2.7,1.22));
#12448=CARTESIAN_POINT('',(14.5,2.7,1.22));
#12449=CARTESIAN_POINT('',(11.,2.7,1.22));
#12450=CARTESIAN_POINT('Origin',(11.,1.83,1.22));
#12451=CARTESIAN_POINT('',(11.,1.83,1.22));
#12452=CARTESIAN_POINT('',(11.,1.83,1.22));
#12453=CARTESIAN_POINT('',(14.5,1.83,1.22));
#12454=CARTESIAN_POINT('',(14.5,1.83,1.22));
#12455=CARTESIAN_POINT('',(11.,1.83,1.22));
#12456=CARTESIAN_POINT('Origin',(11.,2.42,2.4));
#12457=CARTESIAN_POINT('',(11.,2.42,2.4));
#12458=CARTESIAN_POINT('',(14.5,2.42,2.4));
#12459=CARTESIAN_POINT('Origin',(14.5,2.265,1.81));
#12460=CARTESIAN_POINT('Origin',(11.,2.265,1.81));
#12461=CARTESIAN_POINT('',(0.,0.,0.));
#12462=CARTESIAN_POINT('Origin',(14.95,3.75,5.));
#12463=CARTESIAN_POINT('',(11.,3.75,4.6));
#12464=CARTESIAN_POINT('',(11.,3.75,7.));
#12465=CARTESIAN_POINT('',(11.,3.75,4.8));
#12466=CARTESIAN_POINT('',(10.,3.75,4.6));
#12467=CARTESIAN_POINT('',(12.725,3.75,4.6));
#12468=CARTESIAN_POINT('',(10.,3.75,7.));
#12469=CARTESIAN_POINT('',(10.,3.75,4.8));
#12470=CARTESIAN_POINT('',(12.725,3.75,7.));
#12471=CARTESIAN_POINT('Origin',(10.,5.,4.6));
#12472=CARTESIAN_POINT('',(10.,-3.75,4.6));
#12473=CARTESIAN_POINT('',(10.,5.,4.6));
#12474=CARTESIAN_POINT('',(10.,-3.75,7.));
#12475=CARTESIAN_POINT('',(10.,-3.75,4.8));
#12476=CARTESIAN_POINT('',(10.,5.,7.));
#12477=CARTESIAN_POINT('',(10.,3.,6.275));
#12478=CARTESIAN_POINT('Origin',(10.,3.,5.8));
#12479=CARTESIAN_POINT('',(10.,-3.,6.275));
#12480=CARTESIAN_POINT('Origin',(10.,-3.,5.8));
#12481=CARTESIAN_POINT('Origin',(10.5,0.,4.6));
#12482=CARTESIAN_POINT('',(11.,-3.75,4.6));
#12483=CARTESIAN_POINT('',(11.,-5.,4.6));
#12484=CARTESIAN_POINT('',(12.725,-3.75,4.6));
#12485=CARTESIAN_POINT('Origin',(14.95,-3.75,5.));
#12486=CARTESIAN_POINT('',(11.,-3.75,7.));
#12487=CARTESIAN_POINT('',(11.,-3.75,4.8));
#12488=CARTESIAN_POINT('',(12.725,-3.75,7.));
#12489=CARTESIAN_POINT('Origin',(11.,-5.,4.6));
#12490=CARTESIAN_POINT('',(11.,-5.,7.));
#12491=CARTESIAN_POINT('',(11.,3.,6.075));
#12492=CARTESIAN_POINT('Origin',(11.,3.,5.8));
#12493=CARTESIAN_POINT('',(11.,-3.,6.075));
#12494=CARTESIAN_POINT('Origin',(11.,-3.,5.8));
#12495=CARTESIAN_POINT('Origin',(9.9,-3.,5.8));
#12496=CARTESIAN_POINT('',(10.55,-3.,6.275));
#12497=CARTESIAN_POINT('',(9.9,-3.,6.275));
#12498=CARTESIAN_POINT('Origin',(10.55,-3.,5.8));
#12499=CARTESIAN_POINT('Origin',(10.55,-3.,5.8));
#12500=CARTESIAN_POINT('',(10.55,-3.,6.075));
#12501=CARTESIAN_POINT('Origin',(10.55,-3.,5.8));
#12502=CARTESIAN_POINT('Origin',(9.9,3.,5.8));
#12503=CARTESIAN_POINT('',(10.55,3.,6.275));
#12504=CARTESIAN_POINT('',(9.9,3.,6.275));
#12505=CARTESIAN_POINT('Origin',(10.55,3.,5.8));
#12506=CARTESIAN_POINT('Origin',(10.55,3.,5.8));
#12507=CARTESIAN_POINT('',(10.55,3.,6.075));
#12508=CARTESIAN_POINT('Origin',(10.55,3.,5.8));
#12509=CARTESIAN_POINT('Origin',(9.9,-3.,5.8));
#12510=CARTESIAN_POINT('',(9.9,-3.,6.075));
#12511=CARTESIAN_POINT('Origin',(9.9,3.,5.8));
#12512=CARTESIAN_POINT('',(9.9,3.,6.075));
#12513=CARTESIAN_POINT('Origin',(10.5,0.,7.));
#12514=CARTESIAN_POINT('',(0.,0.,0.));
#12515=CARTESIAN_POINT('Origin',(12.5,0.,4.));
#12516=CARTESIAN_POINT('',(12.7800042915148,-1.13874042544416E-5,4.45787212683272));
#12517=CARTESIAN_POINT('',(12.6699957084852,1.09516003635735E-5,4.45788309353564));
#12518=CARTESIAN_POINT('',(12.5,-5.60735153159594E-17,4.457875));
#12519=CARTESIAN_POINT('',(12.5,-0.186196943290586,3.58169363627331));
#12520=CARTESIAN_POINT('Ctrl Pts',(12.6699957084852,1.09516003635735E-5,
4.45788309353564));
#12521=CARTESIAN_POINT('Ctrl Pts',(12.6684300766731,0.0150239422001319,
4.45789815019349));
#12522=CARTESIAN_POINT('Ctrl Pts',(12.6668644448611,0.0300354905662504,
4.45717403092565));
#12523=CARTESIAN_POINT('Ctrl Pts',(12.6652988130491,0.0449730203321769,
4.45569984746698));
#12524=CARTESIAN_POINT('Ctrl Pts',(12.6574274409991,0.120072959788606,4.44828824124903));
#12525=CARTESIAN_POINT('Ctrl Pts',(12.6495560689492,0.193301947984492,4.42191743369942));
#12526=CARTESIAN_POINT('Ctrl Pts',(12.6416846968992,0.255884660534875,4.37974732787395));
#12527=CARTESIAN_POINT('Ctrl Pts',(12.6338133248492,0.318467373085258,4.33757722204849));
#12528=CARTESIAN_POINT('Ctrl Pts',(12.6259419527993,0.370403809990138,4.27960781794716));
#12529=CARTESIAN_POINT('Ctrl Pts',(12.6180705807493,0.405471379329245,4.2127856577826));
#12530=CARTESIAN_POINT('Ctrl Pts',(12.6101992086994,0.440538948668352,4.14596349761803));
#12531=CARTESIAN_POINT('Ctrl Pts',(12.6023278366494,0.458737650441686,4.07028858139023));
#12532=CARTESIAN_POINT('Ctrl Pts',(12.5944564645995,0.457884906392306,3.99482861029462));
#12533=CARTESIAN_POINT('Ctrl Pts',(12.5865850925495,0.457032162342926,3.91936863919901));
#12534=CARTESIAN_POINT('Ctrl Pts',(12.5787137204996,0.437127972470831,3.84412361323559));
#12535=CARTESIAN_POINT('Ctrl Pts',(12.5708423484496,0.400561475243013,3.77811083326841));
#12536=CARTESIAN_POINT('Ctrl Pts',(12.5629709763996,0.363994978015195,3.71209805330123));
#12537=CARTESIAN_POINT('Ctrl Pts',(12.5550996043497,0.310766173431653,3.6553175193303));
#12538=CARTESIAN_POINT('Ctrl Pts',(12.5472282322997,0.247245050961511,3.61457214242492));
#12539=CARTESIAN_POINT('Ctrl Pts',(12.5393568602498,0.183723928491369,3.57382676551955));
#12540=CARTESIAN_POINT('Ctrl Pts',(12.5314854881998,0.109910488134627,3.54911654567973));
#12541=CARTESIAN_POINT('Ctrl Pts',(12.5236141161499,0.034670519197381,3.5434092666393));
#12542=CARTESIAN_POINT('Ctrl Pts',(12.5157427440999,-0.0405694497398647,
3.53770198759887));
#12543=CARTESIAN_POINT('Ctrl Pts',(12.50787137205,-0.117235947257613,3.55099764935784));
#12544=CARTESIAN_POINT('Ctrl Pts',(12.5,-0.186196943290592,3.58169363627332));
#12545=CARTESIAN_POINT('',(12.5,-0.186217277007329,4.41832740439831));
#12546=CARTESIAN_POINT('Origin',(12.5,0.,4.));
#12547=CARTESIAN_POINT('Ctrl Pts',(12.5,-0.186217277007329,4.41832740439831));
#12548=CARTESIAN_POINT('Ctrl Pts',(12.5008157411716,-0.193365324225124,
4.41515241707318));
#12549=CARTESIAN_POINT('Ctrl Pts',(12.5016314823431,-0.200430783441492,
4.4117927098014));
#12550=CARTESIAN_POINT('Ctrl Pts',(12.5024472235147,-0.207403505574881,
4.40825058102053));
#12551=CARTESIAN_POINT('Ctrl Pts',(12.5103185955646,-0.274685741688951,
4.37407134077235));
#12552=CARTESIAN_POINT('Ctrl Pts',(12.5181899676146,-0.333333232193243,
4.32290684204764));
#12553=CARTESIAN_POINT('Ctrl Pts',(12.5260613396645,-0.376326743005614,
4.26088786252735));
#12554=CARTESIAN_POINT('Ctrl Pts',(12.5339327117145,-0.419320253817985,
4.19886888300706));
#12555=CARTESIAN_POINT('Ctrl Pts',(12.5418040837645,-0.446659784938435,
4.12599542269119));
#12556=CARTESIAN_POINT('Ctrl Pts',(12.5496754558144,-0.455065168373522,
4.05100019606997));
#12557=CARTESIAN_POINT('Ctrl Pts',(12.5575468278644,-0.463470551808608,
3.97600496944875));
#12558=CARTESIAN_POINT('Ctrl Pts',(12.5654181999143,-0.452941787558331,
3.89888797652218));
#12559=CARTESIAN_POINT('Ctrl Pts',(12.5732895719643,-0.424742400952558,
3.82888990513641));
#12560=CARTESIAN_POINT('Ctrl Pts',(12.5811609440142,-0.396543014346786,
3.75889183375065));
#12561=CARTESIAN_POINT('Ctrl Pts',(12.5890323160642,-0.350673005385519,
3.69601268390568));
#12562=CARTESIAN_POINT('Ctrl Pts',(12.5969036881141,-0.292628022669152,
3.64778723809593));
#12563=CARTESIAN_POINT('Ctrl Pts',(12.6047750601641,-0.234583039952784,
3.59956179228618));
#12564=CARTESIAN_POINT('Ctrl Pts',(12.6126464322141,-0.164363083481316,
3.56599005051166));
#12565=CARTESIAN_POINT('Ctrl Pts',(12.620517804264,-0.0903829156297007,
3.55109483330951));
#12566=CARTESIAN_POINT('Ctrl Pts',(12.628389176314,-0.0164027477780855,
3.53619961610736));
#12567=CARTESIAN_POINT('Ctrl Pts',(12.6362605483639,0.0613376314536766,
3.53998092347757));
#12568=CARTESIAN_POINT('Ctrl Pts',(12.6441319204139,0.13352290298843,3.56198566164487));
#12569=CARTESIAN_POINT('Ctrl Pts',(12.6520032924638,0.205708174523184,3.58399039981218));
#12570=CARTESIAN_POINT('Ctrl Pts',(12.6598746645138,0.272338338360929,3.62421856877658));
#12571=CARTESIAN_POINT('Ctrl Pts',(12.6677460365637,0.325429113408527,3.67784968145944));
#12572=CARTESIAN_POINT('Ctrl Pts',(12.6756174086137,0.378519888456125,3.7314807941423));
#12573=CARTESIAN_POINT('Ctrl Pts',(12.6834887806637,0.418071274713577,3.79851485054363));
#12574=CARTESIAN_POINT('Ctrl Pts',(12.6913601527136,0.439343931585728,3.87091926467948));
#12575=CARTESIAN_POINT('Ctrl Pts',(12.6992315247636,0.460616588457879,3.94332367881533));
#12576=CARTESIAN_POINT('Ctrl Pts',(12.7071028968135,0.46361051594473,4.02109845068571));
#12577=CARTESIAN_POINT('Ctrl Pts',(12.7149742688635,0.447966936692366,4.09492394607626));
#12578=CARTESIAN_POINT('Ctrl Pts',(12.7228456409134,0.432323357440003,4.16874944146681));
#12579=CARTESIAN_POINT('Ctrl Pts',(12.7307170129634,0.398042271448426,4.23862566037754));
#12580=CARTESIAN_POINT('Ctrl Pts',(12.7385883850133,0.349231538304918,4.29617944234672));
#12581=CARTESIAN_POINT('Ctrl Pts',(12.7464597570633,0.300420805161409,4.35373322431589));
#12582=CARTESIAN_POINT('Ctrl Pts',(12.7543311291133,0.237080424865968,4.39896456934351));
#12583=CARTESIAN_POINT('Ctrl Pts',(12.7622025011632,0.166800374688878,4.42645347375649));
#12584=CARTESIAN_POINT('Ctrl Pts',(12.7681364312804,0.113818899065861,4.4471763206439));
#12585=CARTESIAN_POINT('Ctrl Pts',(12.7740703613976,0.056893551674301,4.45781599184163));
#12586=CARTESIAN_POINT('Ctrl Pts',(12.7800042915148,-1.13874042544416E-5,
4.45787212683272));
#12587=CARTESIAN_POINT('Origin',(12.5,0.,4.));
#12588=CARTESIAN_POINT('',(13.0800042915148,2.8196954984682E-6,4.45783894202495));
#12589=CARTESIAN_POINT('',(12.9699957084852,-6.90274666573233E-6,4.45790451736119));
#12590=CARTESIAN_POINT('',(12.5,-5.60735153159594E-17,4.457875));
#12591=CARTESIAN_POINT('Ctrl Pts',(12.9699957084852,-6.90274666573233E-6,
4.45790451736119));
#12592=CARTESIAN_POINT('Ctrl Pts',(12.9628865412726,0.0681543496286777,
4.45785453236543));
#12593=CARTESIAN_POINT('Ctrl Pts',(12.95577737406,0.136337475731944,4.44242789501186));
#12594=CARTESIAN_POINT('Ctrl Pts',(12.9486682068475,0.197807532932104,4.41298560914613));
#12595=CARTESIAN_POINT('Ctrl Pts',(12.9407968347975,0.265868063186489,4.38038668734267));
#12596=CARTESIAN_POINT('Ctrl Pts',(12.9329254627476,0.325698883531032,4.33060565060516));
#12597=CARTESIAN_POINT('Ctrl Pts',(12.9250540906976,0.370130557623211,4.26960768492436));
#12598=CARTESIAN_POINT('Ctrl Pts',(12.9171827186476,0.41456223171539,4.20860971924356));
#12599=CARTESIAN_POINT('Ctrl Pts',(12.9093113465977,0.443594759555206,4.13639482461947));
#12600=CARTESIAN_POINT('Ctrl Pts',(12.9014399745477,0.453749217534713,4.06161640217293));
#12601=CARTESIAN_POINT('Ctrl Pts',(12.8935686024978,0.463903675514219,3.9868379797264));
#12602=CARTESIAN_POINT('Ctrl Pts',(12.8856972304478,0.455180063633418,3.90949602945742));
#12603=CARTESIAN_POINT('Ctrl Pts',(12.8778258583979,0.428623718850503,3.83885831972366));
#12604=CARTESIAN_POINT('Ctrl Pts',(12.8699544863479,0.402067374067587,3.7682206099899));
#12605=CARTESIAN_POINT('Ctrl Pts',(12.862083114298,0.357678296382559,3.70428714079136));
#12606=CARTESIAN_POINT('Ctrl Pts',(12.854211742248,0.300775561959983,3.65471896268111));
#12607=CARTESIAN_POINT('Ctrl Pts',(12.846340370198,0.243872827537407,3.60515078457087));
#12608=CARTESIAN_POINT('Ctrl Pts',(12.8384689981481,0.174456436377283,3.56994789754891));
#12609=CARTESIAN_POINT('Ctrl Pts',(12.8305976260981,0.100844448250471,3.55332860992135));
#12610=CARTESIAN_POINT('Ctrl Pts',(12.8227262540482,0.0272324601236582,
3.53670932229378));
#12611=CARTESIAN_POINT('Ctrl Pts',(12.8148548819982,-0.0505751249698428,
3.53867363406062));
#12612=CARTESIAN_POINT('Ctrl Pts',(12.8069835099483,-0.123254740362562,
3.558986165072));
#12613=CARTESIAN_POINT('Ctrl Pts',(12.7991121378983,-0.195934355755281,
3.57929869608338));
#12614=CARTESIAN_POINT('Ctrl Pts',(12.7912407658484,-0.263486001447217,
3.6179594463393));
#12615=CARTESIAN_POINT('Ctrl Pts',(12.7833693937984,-0.317815070570116,
3.67033575613656));
#12616=CARTESIAN_POINT('Ctrl Pts',(12.7754980217484,-0.372144139693014,
3.72271206593382));
#12617=CARTESIAN_POINT('Ctrl Pts',(12.7676266496985,-0.413250632246875,
3.78880393527241));
#12618=CARTESIAN_POINT('Ctrl Pts',(12.7597552776485,-0.43620881068128,3.86069167744737));
#12619=CARTESIAN_POINT('Ctrl Pts',(12.7518839055986,-0.459166989115684,
3.93257941962233));
#12620=CARTESIAN_POINT('Ctrl Pts',(12.7440125335486,-0.463976853430633,
4.01026303463365));
#12621=CARTESIAN_POINT('Ctrl Pts',(12.7361411614987,-0.450062064178823,
4.08443380953254));
#12622=CARTESIAN_POINT('Ctrl Pts',(12.7282697894487,-0.436147274927012,
4.15860458443143));
#12623=CARTESIAN_POINT('Ctrl Pts',(12.7203984173988,-0.403507832108441,
4.22926251921788));
#12624=CARTESIAN_POINT('Ctrl Pts',(12.7125270453488,-0.356054829243877,
4.28794078818664));
#12625=CARTESIAN_POINT('Ctrl Pts',(12.7046556732988,-0.308601826379312,
4.3466190571554));
#12626=CARTESIAN_POINT('Ctrl Pts',(12.6967843012489,-0.246335263468753,
4.39331766030646));
#12627=CARTESIAN_POINT('Ctrl Pts',(12.6889129291989,-0.176716536654988,
4.42244075943884));
#12628=CARTESIAN_POINT('Ctrl Pts',(12.682607188961,-0.120945115332726,4.44577121528397));
#12629=CARTESIAN_POINT('Ctrl Pts',(12.6763014487231,-0.0604553842193124,
4.45782245132557));
#12630=CARTESIAN_POINT('Ctrl Pts',(12.6699957084852,1.09516003635735E-5,
4.45788309353564));
#12631=CARTESIAN_POINT('Ctrl Pts',(12.7800042915148,-1.13874042544416E-5,
4.45787212683272));
#12632=CARTESIAN_POINT('Ctrl Pts',(12.7819417334476,-0.0185909818676029,
4.45789045503738));
#12633=CARTESIAN_POINT('Ctrl Pts',(12.7838791753803,-0.0371684007279871,
4.45678053845584));
#12634=CARTESIAN_POINT('Ctrl Pts',(12.7858166173131,-0.0556056617636943,
4.45452496135198));
#12635=CARTESIAN_POINT('Ctrl Pts',(12.793687989363,-0.130511927980435,4.44536108073615));
#12636=CARTESIAN_POINT('Ctrl Pts',(12.801559361413,-0.203104740355178,4.41728685570614));
#12637=CARTESIAN_POINT('Ctrl Pts',(12.8094307334629,-0.264685413403174,
4.37366637792357));
#12638=CARTESIAN_POINT('Ctrl Pts',(12.8173021055129,-0.32626608645117,4.33004590014099));
#12639=CARTESIAN_POINT('Ctrl Pts',(12.8251734775629,-0.37683462017242,4.27087916960585));
#12640=CARTESIAN_POINT('Ctrl Pts',(12.8330448496128,-0.410331463567461,
4.20325604577686));
#12641=CARTESIAN_POINT('Ctrl Pts',(12.8409162216628,-0.443828306962503,
4.13563292194788));
#12642=CARTESIAN_POINT('Ctrl Pts',(12.8487875937127,-0.460253460031337,
4.05955340482505));
#12643=CARTESIAN_POINT('Ctrl Pts',(12.8566589657627,-0.457638721839564,
3.98413398734005));
#12644=CARTESIAN_POINT('Ctrl Pts',(12.8645303378126,-0.45502398364779,3.90871456985506));
#12645=CARTESIAN_POINT('Ctrl Pts',(12.8724017098626,-0.433369354195409,
3.8339552520079));
#12646=CARTESIAN_POINT('Ctrl Pts',(12.8802730819125,-0.395269674734573,
3.76881432927916));
#12647=CARTESIAN_POINT('Ctrl Pts',(12.8881444539625,-0.357169995273737,
3.70367340655041));
#12648=CARTESIAN_POINT('Ctrl Pts',(12.8960158260125,-0.302625265804445,
3.64815087894007));
#12649=CARTESIAN_POINT('Ctrl Pts',(12.9038871980624,-0.238171498431664,
3.6088999265713));
#12650=CARTESIAN_POINT('Ctrl Pts',(12.9117585701124,-0.173717731058884,
3.56964897420252));
#12651=CARTESIAN_POINT('Ctrl Pts',(12.9196299421623,-0.0993549257826154,
3.5466695970753));
#12652=CARTESIAN_POINT('Ctrl Pts',(12.9275013142123,-0.023993864556795,
3.54271537903906));
#12653=CARTESIAN_POINT('Ctrl Pts',(12.9353726862622,0.0513671966690251,
3.53876116100282));
#12654=CARTESIAN_POINT('Ctrl Pts',(12.9432440583122,0.127726513844396,3.55383210205756));
#12655=CARTESIAN_POINT('Ctrl Pts',(12.9511154303621,0.195934065997641,3.58612227423372));
#12656=CARTESIAN_POINT('Ctrl Pts',(12.9589868024121,0.264141618150887,3.61841244640988));
#12657=CARTESIAN_POINT('Ctrl Pts',(12.9668581744621,0.324197405282005,3.66792184970745));
#12658=CARTESIAN_POINT('Ctrl Pts',(12.974729546512,0.368905033668178,3.72871784755079));
#12659=CARTESIAN_POINT('Ctrl Pts',(12.982600918562,0.41361266205435,3.78951384539413));
#12660=CARTESIAN_POINT('Ctrl Pts',(12.9904722906119,0.442972131695578,3.86159643778324));
#12661=CARTESIAN_POINT('Ctrl Pts',(12.9983436626619,0.453465341949404,3.93632807718928));
#12662=CARTESIAN_POINT('Ctrl Pts',(13.0062150347118,0.46395855220323,4.01105971659532));
#12663=CARTESIAN_POINT('Ctrl Pts',(13.0140864067618,0.455585503069655,4.0884404030183));
#12664=CARTESIAN_POINT('Ctrl Pts',(13.0219577788117,0.429349524305901,4.15919772637108));
#12665=CARTESIAN_POINT('Ctrl Pts',(13.0298291508617,0.403113545542148,4.22995504972387));
#12666=CARTESIAN_POINT('Ctrl Pts',(13.0377005229117,0.359014637148215,4.29408901000646));
#12667=CARTESIAN_POINT('Ctrl Pts',(13.0455718949616,0.302337104315659,4.34391453219887));
#12668=CARTESIAN_POINT('Ctrl Pts',(13.0534432670116,0.245659571483104,4.39374005439127));
#12669=CARTESIAN_POINT('Ctrl Pts',(13.0613146390615,0.176403414211925,4.4292571384935));
#12670=CARTESIAN_POINT('Ctrl Pts',(13.0691860111115,0.102867492605122,4.44620982627979));
#12671=CARTESIAN_POINT('Ctrl Pts',(13.0727921045793,0.0691786509558273,
4.45397632191734));
#12672=CARTESIAN_POINT('Ctrl Pts',(13.076398198047,0.0345915681853763,4.45784650391406));
#12673=CARTESIAN_POINT('Ctrl Pts',(13.0800042915148,2.8196954984682E-6,
4.45783894202495));
#12674=CARTESIAN_POINT('Origin',(12.5,0.,4.));
#12675=CARTESIAN_POINT('',(13.3800042915148,1.00338821889499E-5,4.45789143379912));
#12676=CARTESIAN_POINT('',(13.2699957084852,-6.83105689078257E-6,4.45784477598907));
#12677=CARTESIAN_POINT('',(12.5,-5.60735153159594E-17,4.457875));
#12678=CARTESIAN_POINT('Ctrl Pts',(13.2699957084852,-6.83105689078257E-6,
4.45784477598907));
#12679=CARTESIAN_POINT('Ctrl Pts',(13.265214377922,0.0458528260712244,4.45782008288951));
#12680=CARTESIAN_POINT('Ctrl Pts',(13.2604330473589,0.091719698604501,4.45096974854549));
#12681=CARTESIAN_POINT('Ctrl Pts',(13.2556517167957,0.135506404234727,4.43740478719402));
#12682=CARTESIAN_POINT('Ctrl Pts',(13.2477803447458,0.207591244700251,4.41507316710824));
#12683=CARTESIAN_POINT('Ctrl Pts',(13.2399089726958,0.274038390871736,4.37454348113122));
#12684=CARTESIAN_POINT('Ctrl Pts',(13.2320376006459,0.326885582178656,4.32067233995558));
#12685=CARTESIAN_POINT('Ctrl Pts',(13.2241662285959,0.379732773485576,4.26680119877995));
#12686=CARTESIAN_POINT('Ctrl Pts',(13.2162948565459,0.418980009927931,4.19958860240569));
#12687=CARTESIAN_POINT('Ctrl Pts',(13.208423484496,0.439924354792367,4.12708853413817));
#12688=CARTESIAN_POINT('Ctrl Pts',(13.200552112446,0.460868699656804,4.05458846587065));
#12689=CARTESIAN_POINT('Ctrl Pts',(13.1926807403961,0.463510152943321,3.97680092570987));
#12690=CARTESIAN_POINT('Ctrl Pts',(13.1848093683461,0.447532193317848,3.90304707640827));
#12691=CARTESIAN_POINT('Ctrl Pts',(13.1769379962962,0.431554233692375,3.82929322710668));
#12692=CARTESIAN_POINT('Ctrl Pts',(13.1690666242462,0.396956861154912,3.75957306866428));
#12693=CARTESIAN_POINT('Ctrl Pts',(13.1611952521963,0.347885826291745,3.70224106173923));
#12694=CARTESIAN_POINT('Ctrl Pts',(13.1533238801463,0.298814791428577,3.64490905481418));
#12695=CARTESIAN_POINT('Ctrl Pts',(13.1454525080963,0.235270094239705,3.59996519940648));
#12696=CARTESIAN_POINT('Ctrl Pts',(13.1375811360464,0.164866199243897,3.57279504942506));
#12697=CARTESIAN_POINT('Ctrl Pts',(13.1297097639964,0.0944623042480882,
3.54562489944363));
#12698=CARTESIAN_POINT('Ctrl Pts',(13.1218383919465,0.0171992114453437,
3.53622845488849));
#12699=CARTESIAN_POINT('Ctrl Pts',(13.1139670198965,-0.0576647601420857,
3.54573167743434));
#12700=CARTESIAN_POINT('Ctrl Pts',(13.1060956478466,-0.132528731729515,
3.55523489998019));
#12701=CARTESIAN_POINT('Ctrl Pts',(13.0982242757966,-0.204993582101629,
3.58363778962703));
#12702=CARTESIAN_POINT('Ctrl Pts',(13.0903529037467,-0.266375958336211,
3.62753687126191));
#12703=CARTESIAN_POINT('Ctrl Pts',(13.0824815316967,-0.327758334570793,
3.67143595289679));
#12704=CARTESIAN_POINT('Ctrl Pts',(13.0746101596467,-0.378058236667844,
3.73083122651971));
#12705=CARTESIAN_POINT('Ctrl Pts',(13.0667387875968,-0.411248303781717,
3.79860544673343));
#12706=CARTESIAN_POINT('Ctrl Pts',(13.0588674155468,-0.444438370895591,
3.86637966694714));
#12707=CARTESIAN_POINT('Ctrl Pts',(13.0509960434969,-0.460518603026287,
3.94253283375165));
#12708=CARTESIAN_POINT('Ctrl Pts',(13.0431246714469,-0.457562130387816,
4.0179396288708));
#12709=CARTESIAN_POINT('Ctrl Pts',(13.035253299397,-0.454605657749345,4.09334642398995));
#12710=CARTESIAN_POINT('Ctrl Pts',(13.027381927347,-0.432612480341706,4.16800684742375));
#12711=CARTESIAN_POINT('Ctrl Pts',(13.0195105552971,-0.394218007200806,
4.23297445406563));
#12712=CARTESIAN_POINT('Ctrl Pts',(13.0116391832471,-0.355823534059905,
4.29794206070751));
#12713=CARTESIAN_POINT('Ctrl Pts',(13.0037678111972,-0.301027765185743,
4.35321685055749));
#12714=CARTESIAN_POINT('Ctrl Pts',(12.9958964391472,-0.236396794305188,
4.39217532952931));
#12715=CARTESIAN_POINT('Ctrl Pts',(12.9880250670972,-0.171765823424632,
4.43113380850113));
#12716=CARTESIAN_POINT('Ctrl Pts',(12.9801536950473,-0.0972996505376846,
4.45377597659478));
#12717=CARTESIAN_POINT('Ctrl Pts',(12.9722823229973,-0.0219214440120968,
4.4573886572069));
#12718=CARTESIAN_POINT('Ctrl Pts',(12.9715201181599,-0.014622381881285,
4.45773848219561));
#12719=CARTESIAN_POINT('Ctrl Pts',(12.9707579133226,-0.00731476803234869,
4.45790987647069));
#12720=CARTESIAN_POINT('Ctrl Pts',(12.9699957084852,-6.90274666573233E-6,
4.45790451736119));
#12721=CARTESIAN_POINT('Ctrl Pts',(13.0800042915148,2.8196954984682E-6,
4.45783894202495));
#12722=CARTESIAN_POINT('Ctrl Pts',(13.084269570097,-0.0409086678841046,
4.4578299978409));
#12723=CARTESIAN_POINT('Ctrl Pts',(13.0885348486792,-0.0818224858219862,
4.45239605085009));
#12724=CARTESIAN_POINT('Ctrl Pts',(13.0928001272613,-0.121255029803553,
4.44156782927524));
#12725=CARTESIAN_POINT('Ctrl Pts',(13.1006714993113,-0.194025944662995,
4.42158485301405));
#12726=CARTESIAN_POINT('Ctrl Pts',(13.1085428713613,-0.261752088439453,
4.3832306090213));
#12727=CARTESIAN_POINT('Ctrl Pts',(13.1164142434112,-0.31631794022257,4.33110102808186));
#12728=CARTESIAN_POINT('Ctrl Pts',(13.1242856154612,-0.370883792005687,
4.27897144714243));
#12729=CARTESIAN_POINT('Ctrl Pts',(13.1321569875111,-0.412289351795463,
4.21306652925631));
#12730=CARTESIAN_POINT('Ctrl Pts',(13.1400283595611,-0.435573054271055,
4.14128356060242));
#12731=CARTESIAN_POINT('Ctrl Pts',(13.147899731611,-0.458856756746647,4.06950059194853));
#12732=CARTESIAN_POINT('Ctrl Pts',(13.155771103661,-0.464018601908056,3.99183957252686));
#12733=CARTESIAN_POINT('Ctrl Pts',(13.1636424757109,-0.45044005369213,3.91760650430194));
#12734=CARTESIAN_POINT('Ctrl Pts',(13.1715138477609,-0.436861505476204,
3.84337343607703));
#12735=CARTESIAN_POINT('Ctrl Pts',(13.1793852198109,-0.404542563882944,
3.77256831904885));
#12736=CARTESIAN_POINT('Ctrl Pts',(13.1872565918608,-0.357355958580309,
3.7136756228145));
#12737=CARTESIAN_POINT('Ctrl Pts',(13.1951279639108,-0.310169353277673,
3.65478292658016));
#12738=CARTESIAN_POINT('Ctrl Pts',(13.2029993359607,-0.248115084265664,
3.60780265113964));
#12739=CARTESIAN_POINT('Ctrl Pts',(13.2108707080107,-0.178629020319019,
3.57836437152041));
#12740=CARTESIAN_POINT('Ctrl Pts',(13.2187420800606,-0.109142956372374,
3.54892609190117));
#12741=CARTESIAN_POINT('Ctrl Pts',(13.2266134521106,-0.0322250974910928,
3.53702980810322));
#12742=CARTESIAN_POINT('Ctrl Pts',(13.2344848241605,0.0429076061587562,
3.54410103373967));
#12743=CARTESIAN_POINT('Ctrl Pts',(13.2423561962105,0.118040309808605,3.55117225937612));
#12744=CARTESIAN_POINT('Ctrl Pts',(13.2502275682605,0.191387858227023,3.57721099444696));
#12745=CARTESIAN_POINT('Ctrl Pts',(13.2580989403104,0.254161126126225,3.61909705689013));
#12746=CARTESIAN_POINT('Ctrl Pts',(13.2659703123604,0.316934394025428,3.66098311933329));
#12747=CARTESIAN_POINT('Ctrl Pts',(13.2738416844103,0.369133381405416,3.71871650914877));
#12748=CARTESIAN_POINT('Ctrl Pts',(13.2817130564603,0.404503162915977,3.78537912195109));
#12749=CARTESIAN_POINT('Ctrl Pts',(13.2895844285102,0.43987294442654,3.85204173475342));
#12750=CARTESIAN_POINT('Ctrl Pts',(13.2974558005602,0.458413520067676,3.92763357054259));
#12751=CARTESIAN_POINT('Ctrl Pts',(13.3053271726101,0.457903200829578,4.00309657448501));
#12752=CARTESIAN_POINT('Ctrl Pts',(13.3131985446601,0.457392881591479,4.07855957842742));
#12753=CARTESIAN_POINT('Ctrl Pts',(13.3210699167101,0.437831667474148,4.15389375052308));
#12754=CARTESIAN_POINT('Ctrl Pts',(13.32894128876,0.401563549045306,4.22007191138728));
#12755=CARTESIAN_POINT('Ctrl Pts',(13.33681266081,0.365295430616463,4.28625007225149));
#12756=CARTESIAN_POINT('Ctrl Pts',(13.3446840328599,0.31232040787611,4.34327222188425));
#12757=CARTESIAN_POINT('Ctrl Pts',(13.3525554049099,0.248986397312635,4.38430548273058));
#12758=CARTESIAN_POINT('Ctrl Pts',(13.3604267769598,0.185652386749161,4.42533874357692));
#12759=CARTESIAN_POINT('Ctrl Pts',(13.3682981490098,0.111959388362564,4.45038311563682));
#12760=CARTESIAN_POINT('Ctrl Pts',(13.3761695210597,0.0367379221854645,
4.45643756985705));
#12761=CARTESIAN_POINT('Ctrl Pts',(13.3774477778781,0.024522472144774,4.45742077168506));
#12762=CARTESIAN_POINT('Ctrl Pts',(13.3787260346965,0.0122667140672706,
4.45790318029249));
#12763=CARTESIAN_POINT('Ctrl Pts',(13.3800042915148,1.00338821889499E-5,
4.45789143379912));
#12764=CARTESIAN_POINT('Origin',(12.5,0.,4.));
#12765=CARTESIAN_POINT('',(13.6800042915148,-8.85210990424201E-6,4.45789764648838));
#12766=CARTESIAN_POINT('',(13.5699957084852,1.03170790782398E-5,4.4578580083501));
#12767=CARTESIAN_POINT('',(12.5,-5.60735153159594E-17,4.457875));
#12768=CARTESIAN_POINT('Ctrl Pts',(13.5699957084852,1.03170790782398E-5,
4.4578580083501));
#12769=CARTESIAN_POINT('Ctrl Pts',(13.5675422145714,0.0235408097699949,
4.45787795556699));
#12770=CARTESIAN_POINT('Ctrl Pts',(13.5650887206577,0.0470683081483061,
4.45609516914004));
#12771=CARTESIAN_POINT('Ctrl Pts',(13.562635226744,0.0703115975725277,4.45248338388903));
#12772=CARTESIAN_POINT('Ctrl Pts',(13.554763854694,0.144881409096958,4.44089594716616));
#12773=CARTESIAN_POINT('Ctrl Pts',(13.5468924826441,0.21652593236894,4.41048310506186));
#12774=CARTESIAN_POINT('Ctrl Pts',(13.5390211105941,0.276660113016528,4.36488918223832));
#12775=CARTESIAN_POINT('Ctrl Pts',(13.5311497385442,0.336794293664116,4.31929525941478));
#12776=CARTESIAN_POINT('Ctrl Pts',(13.5232783664942,0.385418131687311,4.25852025587201));
#12777=CARTESIAN_POINT('Ctrl Pts',(13.5154069944443,0.416705106451492,4.18984674794718));
#12778=CARTESIAN_POINT('Ctrl Pts',(13.5075356223943,0.447992081215673,4.12117324002235));
#12779=CARTESIAN_POINT('Ctrl Pts',(13.4996642503443,0.461942192720839,4.04460122771548));
#12780=CARTESIAN_POINT('Ctrl Pts',(13.4917928782944,0.456883820300162,3.96930621892307));
#12781=CARTESIAN_POINT('Ctrl Pts',(13.4839215062444,0.451825447879485,3.89401121013066));
#12782=CARTESIAN_POINT('Ctrl Pts',(13.4760501341945,0.427758591532965,3.81999320485271));
#12783=CARTESIAN_POINT('Ctrl Pts',(13.4681787621445,0.387567146091087,3.75612166820384));
#12784=CARTESIAN_POINT('Ctrl Pts',(13.4603073900946,0.347375700649209,3.69225013155497));
#12785=CARTESIAN_POINT('Ctrl Pts',(13.4524360180446,0.291059666111973,3.63852506353517));
#12786=CARTESIAN_POINT('Ctrl Pts',(13.4445646459947,0.225367307335285,3.60138425741911));
#12787=CARTESIAN_POINT('Ctrl Pts',(13.4366932739447,0.159674948558598,3.56424345130305));
#12788=CARTESIAN_POINT('Ctrl Pts',(13.4288219018947,0.0846062655424597,
3.54368690709073));
#12789=CARTESIAN_POINT('Ctrl Pts',(13.4209505298448,0.00915662451852634,
3.54217788424291));
#12790=CARTESIAN_POINT('Ctrl Pts',(13.4130791577948,-0.0662930165054059,
3.54066886139509));
#12791=CARTESIAN_POINT('Ctrl Pts',(13.4052077857449,-0.142123615537132,
3.55820735991178));
#12792=CARTESIAN_POINT('Ctrl Pts',(13.3973364136949,-0.209248507106454,
3.5926917681625));
#12793=CARTESIAN_POINT('Ctrl Pts',(13.389465041645,-0.276373398675776,3.62717617641322));
#12794=CARTESIAN_POINT('Ctrl Pts',(13.381593669595,-0.334792582782693,3.67860649439798));
#12795=CARTESIAN_POINT('Ctrl Pts',(13.3737222975451,-0.377505777353741,
3.74081990525232));
#12796=CARTESIAN_POINT('Ctrl Pts',(13.3658509254951,-0.420218971924789,
3.80303331610666));
#12797=CARTESIAN_POINT('Ctrl Pts',(13.3579795534451,-0.44722617695997,3.87602981983059));
#12798=CARTESIAN_POINT('Ctrl Pts',(13.3501081813952,-0.455291160112798,
3.95106235628872));
#12799=CARTESIAN_POINT('Ctrl Pts',(13.3422368093452,-0.463356143265626,
4.02609489274685));
#12800=CARTESIAN_POINT('Ctrl Pts',(13.3343654372953,-0.452478904536101,
4.10316346193917));
#12801=CARTESIAN_POINT('Ctrl Pts',(13.3264940652453,-0.423962846915058,
4.17303305431203));
#12802=CARTESIAN_POINT('Ctrl Pts',(13.3186226931954,-0.395446789294015,
4.24290264668488));
#12803=CARTESIAN_POINT('Ctrl Pts',(13.3107513211454,-0.349291912781453,
4.30557326223827));
#12804=CARTESIAN_POINT('Ctrl Pts',(13.3028799490955,-0.291028886105345,
4.35353517632783));
#12805=CARTESIAN_POINT('Ctrl Pts',(13.2950085770455,-0.232765859429236,
4.4014970904174));
#12806=CARTESIAN_POINT('Ctrl Pts',(13.2871372049956,-0.162394682589579,
4.43475030304313));
#12807=CARTESIAN_POINT('Ctrl Pts',(13.2792658329456,-0.0883478267899694,
4.44931013225873));
#12808=CARTESIAN_POINT('Ctrl Pts',(13.2761757914588,-0.059279469337623,
4.4550258417985));
#12809=CARTESIAN_POINT('Ctrl Pts',(13.273085749972,-0.0296446570187532,
4.45786073445524));
#12810=CARTESIAN_POINT('Ctrl Pts',(13.2699957084852,-6.83105689078257E-6,
4.45784477598907));
#12811=CARTESIAN_POINT('Ctrl Pts',(13.3800042915148,1.00338821889499E-5,
4.45789143379912));
#12812=CARTESIAN_POINT('Ctrl Pts',(13.3865974067464,-0.0632086430349686,
4.45783084661254));
#12813=CARTESIAN_POINT('Ctrl Pts',(13.393190521978,-0.12645185159805,4.44462381290384));
#12814=CARTESIAN_POINT('Ctrl Pts',(13.3997836372096,-0.184315051738561,
4.41918121595096));
#12815=CARTESIAN_POINT('Ctrl Pts',(13.4076550092596,-0.253396625517876,
4.3888058714441));
#12816=CARTESIAN_POINT('Ctrl Pts',(13.4155263813095,-0.314809839108902,
4.34099064604983));
#12817=CARTESIAN_POINT('Ctrl Pts',(13.4233977533595,-0.361195640434018,
4.28146516557999));
#12818=CARTESIAN_POINT('Ctrl Pts',(13.4312691254094,-0.407581441759134,
4.22193968511016));
#12819=CARTESIAN_POINT('Ctrl Pts',(13.4391404974594,-0.438939830818339,
4.15070394956476));
#12820=CARTESIAN_POINT('Ctrl Pts',(13.4470118695093,-0.451513179494438,
4.07629402890356));
#12821=CARTESIAN_POINT('Ctrl Pts',(13.4548832415593,-0.464086528170537,
4.00188410824235));
#12822=CARTESIAN_POINT('Ctrl Pts',(13.4627546136093,-0.457874836463529,
3.92430000246534));
#12823=CARTESIAN_POINT('Ctrl Pts',(13.4706259856592,-0.433622441953051,
3.85283849709185));
#12824=CARTESIAN_POINT('Ctrl Pts',(13.4784973577092,-0.409370047442573,
3.78137699171835));
#12825=CARTESIAN_POINT('Ctrl Pts',(13.4863687297591,-0.367076950128625,
3.71603808674838));
#12826=CARTESIAN_POINT('Ctrl Pts',(13.4942401018091,-0.311811067605128,
3.66465124389307));
#12827=CARTESIAN_POINT('Ctrl Pts',(13.502111473859,-0.25654518508163,3.61326440103776));
#12828=CARTESIAN_POINT('Ctrl Pts',(13.509982845909,-0.188306517348584,3.5758296202971));
#12829=CARTESIAN_POINT('Ctrl Pts',(13.5178542179589,-0.115272000283325,
3.55683265457144));
#12830=CARTESIAN_POINT('Ctrl Pts',(13.5257255900089,-0.0422374832180674,
3.53783568884578));
#12831=CARTESIAN_POINT('Ctrl Pts',(13.5335969620589,0.035592883179403,3.53727653813511));
#12832=CARTESIAN_POINT('Ctrl Pts',(13.5414683341088,0.108892804353757,3.55522220461956));
#12833=CARTESIAN_POINT('Ctrl Pts',(13.5493397061588,0.182192725528112,3.573167871104));
#12834=CARTESIAN_POINT('Ctrl Pts',(13.5572110782087,0.250962201479351,3.60961835478357));
#12835=CARTESIAN_POINT('Ctrl Pts',(13.5650824502587,0.306960690387823,3.66020584957927));
#12836=CARTESIAN_POINT('Ctrl Pts',(13.5729538223086,0.362959179296295,3.71079334437498));
#12837=CARTESIAN_POINT('Ctrl Pts',(13.5808251943586,0.406186681162,3.77551785028682));
#12838=CARTESIAN_POINT('Ctrl Pts',(13.5886965664085,0.431463310113251,3.84662352810933));
#12839=CARTESIAN_POINT('Ctrl Pts',(13.5965679384585,0.456739939064502,3.91772920593184));
#12840=CARTESIAN_POINT('Ctrl Pts',(13.6044393105085,0.464065695101298,3.99521605566501));
#12841=CARTESIAN_POINT('Ctrl Pts',(13.6123106825584,0.452562744007997,4.06979894583348));
#12842=CARTESIAN_POINT('Ctrl Pts',(13.6201820546084,0.441059792914696,4.14438183600196));
#12843=CARTESIAN_POINT('Ctrl Pts',(13.6280534266583,0.410728134691299,4.21606076660573));
#12844=CARTESIAN_POINT('Ctrl Pts',(13.6359247987083,0.365202365858889,4.27624656029457));
#12845=CARTESIAN_POINT('Ctrl Pts',(13.6437961707582,0.319676597026479,4.33643235398341));
#12846=CARTESIAN_POINT('Ctrl Pts',(13.6516675428082,0.258956717585058,4.38512501075732));
#12847=CARTESIAN_POINT('Ctrl Pts',(13.6595389148581,0.190318698434502,4.41648976353532));
#12848=CARTESIAN_POINT('Ctrl Pts',(13.666360707077,0.130832969391341,4.44367229602021));
#12849=CARTESIAN_POINT('Ctrl Pts',(13.6731824992959,0.065399948454096,4.45783988979956));
#12850=CARTESIAN_POINT('Ctrl Pts',(13.6800042915148,-8.85210990424201E-6,
4.45789764648838));
#12851=CARTESIAN_POINT('Origin',(12.5,0.,4.));
#12852=CARTESIAN_POINT('',(13.9800042915148,-4.68615130337092E-6,4.45784092071359));
#12853=CARTESIAN_POINT('',(13.8699957084852,1.23414887176878E-6,4.4579133809027));
#12854=CARTESIAN_POINT('',(12.5,-5.60735153159594E-17,4.457875));
#12855=CARTESIAN_POINT('Ctrl Pts',(13.8699957084852,1.23414887176878E-6,
4.4579133809027));
#12856=CARTESIAN_POINT('Ctrl Pts',(13.8698700512209,0.00120594270822336,
4.45791357044259));
#12857=CARTESIAN_POINT('Ctrl Pts',(13.8697443939566,0.00241064979645091,
4.45790891401425));
#12858=CARTESIAN_POINT('Ctrl Pts',(13.8696187366923,0.00361531855258033,
4.45789940262096));
#12859=CARTESIAN_POINT('Ctrl Pts',(13.8617473646423,0.0790776965455978,
4.45730359373015));
#12860=CARTESIAN_POINT('Ctrl Pts',(13.8538759925924,0.154389660535011,4.43765704798318));
#12861=CARTESIAN_POINT('Ctrl Pts',(13.8460046205424,0.22052669229976,4.40131398110731));
#12862=CARTESIAN_POINT('Ctrl Pts',(13.8381332484924,0.286663724064511,4.36497091423144));
#12863=CARTESIAN_POINT('Ctrl Pts',(13.8302618764425,0.343625823604597,4.31193132622667));
#12864=CARTESIAN_POINT('Ctrl Pts',(13.8223905043925,0.384587309076409,4.24855087033892));
#12865=CARTESIAN_POINT('Ctrl Pts',(13.8145191323426,0.42554879454822,4.18517041445118));
#12866=CARTESIAN_POINT('Ctrl Pts',(13.8066477602926,0.450509665951756,4.11144909068046));
#12867=CARTESIAN_POINT('Ctrl Pts',(13.7987763882427,0.456478899990553,4.03622081324714));
#12868=CARTESIAN_POINT('Ctrl Pts',(13.7909050161927,0.46244813402935,3.96099253581381));
#12869=CARTESIAN_POINT('Ctrl Pts',(13.7830336441427,0.449425730703409,3.88425730471787));
#12870=CARTESIAN_POINT('Ctrl Pts',(13.7751622720928,0.418972144817937,3.81521018611534));
#12871=CARTESIAN_POINT('Ctrl Pts',(13.7672909000428,0.388518558932466,3.74616306751281));
#12872=CARTESIAN_POINT('Ctrl Pts',(13.7594195279929,0.340633790487464,3.68480406140369));
#12873=CARTESIAN_POINT('Ctrl Pts',(13.7515481559429,0.281055798532888,3.6384857242654));
#12874=CARTESIAN_POINT('Ctrl Pts',(13.743676783893,0.221477806578313,3.59216738712712));
#12875=CARTESIAN_POINT('Ctrl Pts',(13.735805411843,0.150206591114165,3.56088971895966));
#12876=CARTESIAN_POINT('Ctrl Pts',(13.7279340397931,0.0757824736049535,
3.54840067521841));
#12877=CARTESIAN_POINT('Ctrl Pts',(13.7200626677431,0.00135835609574232,
3.53591163147717));
#12878=CARTESIAN_POINT('Ctrl Pts',(13.7121912956931,-0.0762186634585312,
3.54221121216214));
#12879=CARTESIAN_POINT('Ctrl Pts',(13.7043199236432,-0.14765264866984,3.56654454809098));
#12880=CARTESIAN_POINT('Ctrl Pts',(13.6964485515932,-0.219086633881149,
3.59087788401983));
#12881=CARTESIAN_POINT('Ctrl Pts',(13.6885771795433,-0.284377584749494,
3.63324497519255));
#12882=CARTESIAN_POINT('Ctrl Pts',(13.6807058074933,-0.335701785830877,
3.68856903744356));
#12883=CARTESIAN_POINT('Ctrl Pts',(13.6728344354434,-0.38702598691226,3.74389309969457));
#12884=CARTESIAN_POINT('Ctrl Pts',(13.6649630633934,-0.424383438206683,
3.81217413302386));
#12885=CARTESIAN_POINT('Ctrl Pts',(13.6570916913435,-0.443297653083863,
3.88523012494906));
#12886=CARTESIAN_POINT('Ctrl Pts',(13.6492203192935,-0.462211867961044,
3.95828611687427));
#12887=CARTESIAN_POINT('Ctrl Pts',(13.6413489472436,-0.462682846420982,
4.03611706739538));
#12888=CARTESIAN_POINT('Ctrl Pts',(13.6334775751936,-0.444654151830396,
4.10939661196244));
#12889=CARTESIAN_POINT('Ctrl Pts',(13.6256062031436,-0.42662545723981,4.18267615652949));
#12890=CARTESIAN_POINT('Ctrl Pts',(13.6177348310937,-0.3900970895987,4.25140429514248));
#12891=CARTESIAN_POINT('Ctrl Pts',(13.6098634590437,-0.339446187702822,
4.3073454393722));
#12892=CARTESIAN_POINT('Ctrl Pts',(13.6019920869938,-0.288795285806945,
4.36328658360191));
#12893=CARTESIAN_POINT('Ctrl Pts',(13.5941207149438,-0.224021849656302,
4.40644073344835));
#12894=CARTESIAN_POINT('Ctrl Pts',(13.5862493428939,-0.152887581692542,
4.43163679270085));
#12895=CARTESIAN_POINT('Ctrl Pts',(13.5808314647576,-0.103925749791867,
4.44897928111035));
#12896=CARTESIAN_POINT('Ctrl Pts',(13.5754135866214,-0.0519504158054226,
4.45781396031326));
#12897=CARTESIAN_POINT('Ctrl Pts',(13.5699957084852,1.03170790782398E-5,
4.4578580083501));
#12898=CARTESIAN_POINT('Ctrl Pts',(13.6800042915148,-8.85210990424201E-6,
4.45789764648838));
#12899=CARTESIAN_POINT('Ctrl Pts',(13.6810538713459,-0.010072447664127,
4.45790653275371));
#12900=CARTESIAN_POINT('Ctrl Pts',(13.6821034511769,-0.0201354698749596,
4.45758141170421));
#12901=CARTESIAN_POINT('Ctrl Pts',(13.683153031008,-0.0301761699425476,
4.45691829561871));
#12902=CARTESIAN_POINT('Ctrl Pts',(13.691024403058,-0.105476860309351,4.45194522614199));
#12903=CARTESIAN_POINT('Ctrl Pts',(13.6988957751079,-0.179522082183268,
4.42796223840642));
#12904=CARTESIAN_POINT('Ctrl Pts',(13.7067671471579,-0.24343910912634,4.38784317739428));
#12905=CARTESIAN_POINT('Ctrl Pts',(13.7146385192078,-0.307356136069411,
4.34772411638213));
#12906=CARTESIAN_POINT('Ctrl Pts',(13.7225098912578,-0.361144968081636,
4.2914689820934));
#12907=CARTESIAN_POINT('Ctrl Pts',(13.7303812633077,-0.398360171146024,
4.22581874179975));
#12908=CARTESIAN_POINT('Ctrl Pts',(13.7382526353577,-0.435575374210412,
4.1601685015061));
#12909=CARTESIAN_POINT('Ctrl Pts',(13.7461240074077,-0.456216948326962,
4.08512315520753));
#12910=CARTESIAN_POINT('Ctrl Pts',(13.7539953794576,-0.457811445030669,
4.00967527273228));
#12911=CARTESIAN_POINT('Ctrl Pts',(13.7618667515076,-0.459405941734377,
3.93422739025703));
#12912=CARTESIAN_POINT('Ctrl Pts',(13.7697381235575,-0.441953361025241,
3.85837697160509));
#12913=CARTESIAN_POINT('Ctrl Pts',(13.7776094956075,-0.407545019133394,
3.79121305720166));
#12914=CARTESIAN_POINT('Ctrl Pts',(13.7854808676574,-0.373136677241547,
3.72404914279823));
#12915=CARTESIAN_POINT('Ctrl Pts',(13.7933522397074,-0.321772574166988,
3.6655717326433));
#12916=CARTESIAN_POINT('Ctrl Pts',(13.8012236117573,-0.259607592342073,
3.6227880859492));
#12917=CARTESIAN_POINT('Ctrl Pts',(13.8090949838073,-0.19744261051716,3.5800044392551));
#12918=CARTESIAN_POINT('Ctrl Pts',(13.8169663558573,-0.124476749941891,
3.55291455602183));
#12919=CARTESIAN_POINT('Ctrl Pts',(13.8248377279072,-0.0494533988297167,
3.54476457579874));
#12920=CARTESIAN_POINT('Ctrl Pts',(13.8327090999572,0.0255699522824598,
3.53661459557564));
#12921=CARTESIAN_POINT('Ctrl Pts',(13.8405804720071,0.102650793931542,3.54740451836272));
#12922=CARTESIAN_POINT('Ctrl Pts',(13.8484518440571,0.172552645974024,3.57584140410587));
#12923=CARTESIAN_POINT('Ctrl Pts',(13.856323216107,0.242454498016503,3.60427828984902));
#12924=CARTESIAN_POINT('Ctrl Pts',(13.864194588157,0.305177360452382,3.65036213854823));
#12925=CARTESIAN_POINT('Ctrl Pts',(13.8720659602069,0.353205247972751,3.70857079263049));
#12926=CARTESIAN_POINT('Ctrl Pts',(13.8799373322569,0.40123313549312,3.76677944671275));
#12927=CARTESIAN_POINT('Ctrl Pts',(13.8878087043068,0.434566048097978,3.83711290617806));
#12928=CARTESIAN_POINT('Ctrl Pts',(13.8956800763568,0.44920975351361,3.9111432194385));
#12929=CARTESIAN_POINT('Ctrl Pts',(13.9035514484068,0.463853458929242,3.98517353269893));
#12930=CARTESIAN_POINT('Ctrl Pts',(13.9114228204567,0.459807957155645,4.06290069975448));
#12931=CARTESIAN_POINT('Ctrl Pts',(13.9192941925067,0.437558014523894,4.13501079227018));
#12932=CARTESIAN_POINT('Ctrl Pts',(13.9271655645566,0.415308071892144,4.20712088478587));
#12933=CARTESIAN_POINT('Ctrl Pts',(13.9350369366066,0.374853688402242,4.27361390276169));
#12934=CARTESIAN_POINT('Ctrl Pts',(13.9429083086565,0.321042451364188,4.32652208887851));
#12935=CARTESIAN_POINT('Ctrl Pts',(13.9507796807065,0.267231214326134,4.37943027499533));
#12936=CARTESIAN_POINT('Ctrl Pts',(13.9586510527564,0.200063123739928,4.41875362925314));
#12937=CARTESIAN_POINT('Ctrl Pts',(13.9665224248064,0.127586829849962,4.43978009385641));
#12938=CARTESIAN_POINT('Ctrl Pts',(13.9710163803759,0.086208370984788,4.45178460807712));
#12939=CARTESIAN_POINT('Ctrl Pts',(13.9755103359454,0.0430996806131821,
4.45782517307841));
#12940=CARTESIAN_POINT('Ctrl Pts',(13.9800042915148,-4.68615130337092E-6,
4.45784092071359));
#12941=CARTESIAN_POINT('Origin',(12.5,0.,4.));
#12942=CARTESIAN_POINT('',(14.2800042915148,1.11332528513013E-5,4.45786561359635));
#12943=CARTESIAN_POINT('',(14.1699957084852,-1.10604184835328E-5,4.4578646218584));
#12944=CARTESIAN_POINT('',(12.5,-5.60735153159594E-17,4.457875));
#12945=CARTESIAN_POINT('Ctrl Pts',(14.1699957084852,-1.10604184835328E-5,
4.4578646218584));
#12946=CARTESIAN_POINT('Ctrl Pts',(14.1643265158203,0.0543576752587709,
4.45781404039958));
#12947=CARTESIAN_POINT('Ctrl Pts',(14.1586573231555,0.108743966382031,4.44812254260427));
#12948=CARTESIAN_POINT('Ctrl Pts',(14.1529881304907,0.159684023833442,4.42916890146099));
#12949=CARTESIAN_POINT('Ctrl Pts',(14.1451167584407,0.230411580321883,4.40285278028461));
#12950=CARTESIAN_POINT('Ctrl Pts',(14.1372453863907,0.294495541512382,4.358681244225));
#12951=CARTESIAN_POINT('Ctrl Pts',(14.1293740143408,0.344256823700223,4.30194730133701));
#12952=CARTESIAN_POINT('Ctrl Pts',(14.1215026422908,0.394018105888063,4.24521335844902));
#12953=CARTESIAN_POINT('Ctrl Pts',(14.1136312702409,0.429456709073245,4.17591700873265));
#12954=CARTESIAN_POINT('Ctrl Pts',(14.1057598981909,0.446326079279053,4.10236192849032));
#12955=CARTESIAN_POINT('Ctrl Pts',(14.097888526141,0.46319544948486,4.02880684824799));
#12956=CARTESIAN_POINT('Ctrl Pts',(14.090017154091,0.461495586711293,3.95099303747972));
#12957=CARTESIAN_POINT('Ctrl Pts',(14.0821457820411,0.441430182931853,3.87824480690492));
#12958=CARTESIAN_POINT('Ctrl Pts',(14.0742744099911,0.421364779152413,3.80549657633012));
#12959=CARTESIAN_POINT('Ctrl Pts',(14.0664030379411,0.3829338343671,3.73781392594881));
#12960=CARTESIAN_POINT('Ctrl Pts',(14.0585316658912,0.330742470300218,3.68330716492384));
#12961=CARTESIAN_POINT('Ctrl Pts',(14.0506602938412,0.278551106233337,3.62880040389886));
#12962=CARTESIAN_POINT('Ctrl Pts',(14.0427889217913,0.212599322884887,3.58746953223022));
#12963=CARTESIAN_POINT('Ctrl Pts',(14.0349175497413,0.140790022250932,3.5642671654747));
#12964=CARTESIAN_POINT('Ctrl Pts',(14.0270461776914,0.0689807216169763,
3.54106479871918));
#12965=CARTESIAN_POINT('Ctrl Pts',(14.0191748056414,-0.00868609630248519,
3.53599093687678));
#12966=CARTESIAN_POINT('Ctrl Pts',(14.0113034335915,-0.0829037347177578,
3.5496535731032));
#12967=CARTESIAN_POINT('Ctrl Pts',(14.0034320615415,-0.15712137313303,3.56331620932962));
#12968=CARTESIAN_POINT('Ctrl Pts',(13.9955606894916,-0.227889832044114,
3.59571534362485));
#12969=CARTESIAN_POINT('Ctrl Pts',(13.9876893174416,-0.286729034540398,
3.64296863695132));
#12970=CARTESIAN_POINT('Ctrl Pts',(13.9798179453916,-0.345568237036683,
3.69022193027778));
#12971=CARTESIAN_POINT('Ctrl Pts',(13.9719465733417,-0.392478183118168,
3.75232938263547));
#12972=CARTESIAN_POINT('Ctrl Pts',(13.9640752012917,-0.421837725217638,
3.82184875237013));
#12973=CARTESIAN_POINT('Ctrl Pts',(13.9562038292418,-0.451197267317109,
3.8913681221048));
#12974=CARTESIAN_POINT('Ctrl Pts',(13.9483324571918,-0.463006405434566,
3.96829940921644));
#12975=CARTESIAN_POINT('Ctrl Pts',(13.9404610851419,-0.455850068491383,
4.04342405445454));
#12976=CARTESIAN_POINT('Ctrl Pts',(13.9325897130919,-0.448693731548199,
4.11854869969265));
#12977=CARTESIAN_POINT('Ctrl Pts',(13.924718341042,-0.422571919544373,4.19186670305722));
#12978=CARTESIAN_POINT('Ctrl Pts',(13.916846968992,-0.38061476952465,4.25459247959939));
#12979=CARTESIAN_POINT('Ctrl Pts',(13.908975596942,-0.338657619504927,4.31731825614156));
#12980=CARTESIAN_POINT('Ctrl Pts',(13.9011042248921,-0.280865131469307,
4.36945180586132));
#12981=CARTESIAN_POINT('Ctrl Pts',(13.8932328528421,-0.214162491453186,
4.40474604470388));
#12982=CARTESIAN_POINT('Ctrl Pts',(13.8854871380565,-0.148524681204106,
4.43947685223224));
#12983=CARTESIAN_POINT('Ctrl Pts',(13.8777414232708,-0.0742589286223064,
4.45790169736071));
#12984=CARTESIAN_POINT('Ctrl Pts',(13.8699957084852,1.23414887176878E-6,
4.4579133809027));
#12985=CARTESIAN_POINT('Ctrl Pts',(13.9800042915148,-4.68615130337092E-6,
4.45784092071359));
#12986=CARTESIAN_POINT('Ctrl Pts',(13.9833817079953,-0.0323996211791616,
4.45785275579335));
#12987=CARTESIAN_POINT('Ctrl Pts',(13.9867591244758,-0.064792114138131,
4.45446164082457));
#12988=CARTESIAN_POINT('Ctrl Pts',(13.9901365409563,-0.0964458636128916,
4.44764173788363));
#12989=CARTESIAN_POINT('Ctrl Pts',(13.9980079130062,-0.170217765992045,
4.43174734235885));
#12990=CARTESIAN_POINT('Ctrl Pts',(14.0058792850562,-0.239977073556624,
4.39722897636055));
#12991=CARTESIAN_POINT('Ctrl Pts',(14.0137506571061,-0.297364634468633,
4.34822292324149));
#12992=CARTESIAN_POINT('Ctrl Pts',(14.0216220291561,-0.354752195380644,
4.29921687012243));
#12993=CARTESIAN_POINT('Ctrl Pts',(14.0294934012061,-0.399768009640084,
4.23572312988262));
#12994=CARTESIAN_POINT('Ctrl Pts',(14.037364773256,-0.427017900618165,4.16535006094698));
#12995=CARTESIAN_POINT('Ctrl Pts',(14.045236145306,-0.454267791596245,4.09497699201134));
#12996=CARTESIAN_POINT('Ctrl Pts',(14.0531075173559,-0.463751759292965,
4.01772459437987));
#12997=CARTESIAN_POINT('Ctrl Pts',(14.0609788894059,-0.45433335426851,3.94284990548881));
#12998=CARTESIAN_POINT('Ctrl Pts',(14.0688502614558,-0.444914949244056,
3.86797521659775));
#12999=CARTESIAN_POINT('Ctrl Pts',(14.0767216335058,-0.416594171498428,
3.7954782364471));
#13000=CARTESIAN_POINT('Ctrl Pts',(14.0845930055557,-0.372764656800254,
3.7340461680214));
#13001=CARTESIAN_POINT('Ctrl Pts',(14.0924643776057,-0.328935142102078,
3.67261409959569));
#13002=CARTESIAN_POINT('Ctrl Pts',(14.1003357496557,-0.269596890451354,
3.62224694289495));
#13003=CARTESIAN_POINT('Ctrl Pts',(14.1082071217056,-0.201860314388951,
3.58898011778223));
#13004=CARTESIAN_POINT('Ctrl Pts',(14.1160784937556,-0.134123738326549,
3.55571329266952));
#13005=CARTESIAN_POINT('Ctrl Pts',(14.1239498658055,-0.0579888378524715,
3.53954679914483));
#13006=CARTESIAN_POINT('Ctrl Pts',(14.1318212378555,0.0174212575835846,
3.54241784356498));
#13007=CARTESIAN_POINT('Ctrl Pts',(14.1396926099054,0.0928313530196406,
3.54528888798513));
#13008=CARTESIAN_POINT('Ctrl Pts',(14.1475639819554,0.167516643417675,3.56719747035013));
#13009=CARTESIAN_POINT('Ctrl Pts',(14.1554353540053,0.232527703900953,3.60551831852155));
#13010=CARTESIAN_POINT('Ctrl Pts',(14.1633067260553,0.297538764384231,3.64383916669297));
#13011=CARTESIAN_POINT('Ctrl Pts',(14.1711780981053,0.352875594952755,3.69857228067082));
#13012=CARTESIAN_POINT('Ctrl Pts',(14.1790494701552,0.391907267274456,3.76315907456484));
#13013=CARTESIAN_POINT('Ctrl Pts',(14.1869208422052,0.430938939596158,3.82774586845886));
#13014=CARTESIAN_POINT('Ctrl Pts',(14.1947922142551,0.453665453671035,3.90218634226906));
#13015=CARTESIAN_POINT('Ctrl Pts',(14.2026635863051,0.45736352584659,3.97756040711846));
#13016=CARTESIAN_POINT('Ctrl Pts',(14.210534958355,0.461061598022145,4.05293447196787));
#13017=CARTESIAN_POINT('Ctrl Pts',(14.218406330405,0.445731228298378,4.12924212785648));
#13018=CARTESIAN_POINT('Ctrl Pts',(14.2262777024549,0.413209431587385,4.19733954431574));
#13019=CARTESIAN_POINT('Ctrl Pts',(14.2341490745049,0.380687634876391,4.265436960775));
#13020=CARTESIAN_POINT('Ctrl Pts',(14.2420204465549,0.330974411178171,4.32532413780492));
#13021=CARTESIAN_POINT('Ctrl Pts',(14.2498918186048,0.270026820557645,4.36982488597043));
#13022=CARTESIAN_POINT('Ctrl Pts',(14.2577631906548,0.209079229937118,4.41432563413594));
#13023=CARTESIAN_POINT('Ctrl Pts',(14.2656345627047,0.136897272394287,4.44343995343705));
#13024=CARTESIAN_POINT('Ctrl Pts',(14.2735059347547,0.0621304022332317,
4.45367911922619));
#13025=CARTESIAN_POINT('Ctrl Pts',(14.2756720536747,0.0415553447945806,
4.4564968301158));
#13026=CARTESIAN_POINT('Ctrl Pts',(14.2778381725948,0.020784533837212,4.45788513960506));
#13027=CARTESIAN_POINT('Ctrl Pts',(14.2800042915148,1.11332528513013E-5,
4.45786561359635));
#13028=CARTESIAN_POINT('Origin',(12.5,0.,4.));
#13029=CARTESIAN_POINT('',(14.5800042915148,-1.58578451148518E-6,4.45791318879952));
#13030=CARTESIAN_POINT('',(14.4699957084852,4.96934848862042E-6,4.4578413260902));
#13031=CARTESIAN_POINT('',(12.5,-5.60735153159594E-17,4.457875));
#13032=CARTESIAN_POINT('Ctrl Pts',(14.4699957084852,4.96934848862042E-6,
4.4578413260902));
#13033=CARTESIAN_POINT('Ctrl Pts',(14.4666543524698,0.0320539454002899,
4.45785375637851));
#13034=CARTESIAN_POINT('Ctrl Pts',(14.4633129964543,0.0641003838712636,
4.45453523052653));
#13035=CARTESIAN_POINT('Ctrl Pts',(14.4599716404389,0.0954313752779353,
4.44785911407655));
#13036=CARTESIAN_POINT('Ctrl Pts',(14.452100268389,0.169239101517837,4.43213190746217));
#13037=CARTESIAN_POINT('Ctrl Pts',(14.444228896339,0.2390764403586,4.39777168651743));
#13038=CARTESIAN_POINT('Ctrl Pts',(14.4363575242891,0.296574889592956,4.34889578431359));
#13039=CARTESIAN_POINT('Ctrl Pts',(14.4284861522391,0.354073338827311,4.30001988210975));
#13040=CARTESIAN_POINT('Ctrl Pts',(14.4206147801891,0.39923289845526,4.2366282986468));
#13041=CARTESIAN_POINT('Ctrl Pts',(14.4127434081392,0.4266421670589,4.16631715105832));
#13042=CARTESIAN_POINT('Ctrl Pts',(14.4048720360892,0.454051435662541,4.09600600346984));
#13043=CARTESIAN_POINT('Ctrl Pts',(14.3970006640393,0.463710413241873,4.01877529175582));
#13044=CARTESIAN_POINT('Ctrl Pts',(14.3891292919893,0.454461679188747,3.94387945476197));
#13045=CARTESIAN_POINT('Ctrl Pts',(14.3812579199394,0.445212945135621,3.86898361776811));
#13046=CARTESIAN_POINT('Ctrl Pts',(14.3733865478894,0.417056499450037,3.79642265549441));
#13047=CARTESIAN_POINT('Ctrl Pts',(14.3655151758395,0.373366286239542,3.73489143780602));
#13048=CARTESIAN_POINT('Ctrl Pts',(14.3576438037895,0.329676073029047,3.67336022011762));
#13049=CARTESIAN_POINT('Ctrl Pts',(14.3497724317395,0.270452092293641,3.62285874701452));
#13050=CARTESIAN_POINT('Ctrl Pts',(14.3419010596896,0.202791063664024,3.58943853329022));
#13051=CARTESIAN_POINT('Ctrl Pts',(14.3340296876396,0.135130035034407,3.55601831956592));
#13052=CARTESIAN_POINT('Ctrl Pts',(14.3261583155897,0.0590319585105798,
3.53967936522043));
#13053=CARTESIAN_POINT('Ctrl Pts',(14.3182869435397,-0.0163844490157649,
3.54237954232867));
#13054=CARTESIAN_POINT('Ctrl Pts',(14.3104155714898,-0.0918008565421096,
3.54507971943691));
#13055=CARTESIAN_POINT('Ctrl Pts',(14.3025441994398,-0.166535595070972,
3.56681902799889));
#13056=CARTESIAN_POINT('Ctrl Pts',(14.2946728273899,-0.231633314431234,
3.60499247969884));
#13057=CARTESIAN_POINT('Ctrl Pts',(14.2868014553399,-0.296731033791496,
3.64316593139879));
#13058=CARTESIAN_POINT('Ctrl Pts',(14.2789300832899,-0.352191733983158,
3.6977735262367));
#13059=CARTESIAN_POINT('Ctrl Pts',(14.27105871124,-0.391369643565407,3.76227171909014));
#13060=CARTESIAN_POINT('Ctrl Pts',(14.26318733919,-0.430547553147657,3.82676991194359));
#13061=CARTESIAN_POINT('Ctrl Pts',(14.2553159671401,-0.453442672120494,
3.90115870281258));
#13062=CARTESIAN_POINT('Ctrl Pts',(14.2474445950901,-0.457311513162664,
3.97652419590847));
#13063=CARTESIAN_POINT('Ctrl Pts',(14.2395732230402,-0.461180354204834,
4.05188968900435));
#13064=CARTESIAN_POINT('Ctrl Pts',(14.2317018509902,-0.446022917316338,
4.12823188432714));
#13065=CARTESIAN_POINT('Ctrl Pts',(14.2238304789403,-0.413655495130362,
4.19640281260034));
#13066=CARTESIAN_POINT('Ctrl Pts',(14.2159591068903,-0.381288072944386,
4.26457374087354));
#13067=CARTESIAN_POINT('Ctrl Pts',(14.2080877348403,-0.33171066546093,4.32457340209717));
#13068=CARTESIAN_POINT('Ctrl Pts',(14.2002163627904,-0.270864058094251,
4.36921212802613));
#13069=CARTESIAN_POINT('Ctrl Pts',(14.1923449907404,-0.210017450727571,
4.41385085395509));
#13070=CARTESIAN_POINT('Ctrl Pts',(14.1844736186905,-0.137901643477669,
4.44312864458938));
#13071=CARTESIAN_POINT('Ctrl Pts',(14.1766022466405,-0.0631581639595259,
4.45353718675995));
#13072=CARTESIAN_POINT('Ctrl Pts',(14.1744000672554,-0.0422471272657682,
4.45644919204336));
#13073=CARTESIAN_POINT('Ctrl Pts',(14.1721978878703,-0.021130418320356,
4.45788427006097));
#13074=CARTESIAN_POINT('Ctrl Pts',(14.1699957084852,-1.10604184835328E-5,
4.4578646218584));
#13075=CARTESIAN_POINT('Ctrl Pts',(14.2800042915148,1.11332528513013E-5,
4.45786561359635));
#13076=CARTESIAN_POINT('Ctrl Pts',(14.2857095446447,-0.0547030874695854,
4.45781418483069));
#13077=CARTESIAN_POINT('Ctrl Pts',(14.2914147977746,-0.109435272994953,
4.44799629651036));
#13078=CARTESIAN_POINT('Ctrl Pts',(14.2971200509045,-0.16065599949712,4.42880599334559));
#13079=CARTESIAN_POINT('Ctrl Pts',(14.3049914229545,-0.231323748287136,
4.40232968939868));
#13080=CARTESIAN_POINT('Ctrl Pts',(14.3128627950045,-0.295307463087888,
4.35801306922771));
#13081=CARTESIAN_POINT('Ctrl Pts',(14.3207341670544,-0.344940072567234,
4.30116652609615));
#13082=CARTESIAN_POINT('Ctrl Pts',(14.3286055391044,-0.394572682046581,
4.24431998296459));
#13083=CARTESIAN_POINT('Ctrl Pts',(14.3364769111543,-0.429854186204522,
4.17494351687244));
#13084=CARTESIAN_POINT('Ctrl Pts',(14.3443482832043,-0.446556856002091,
4.10135040434572));
#13085=CARTESIAN_POINT('Ctrl Pts',(14.3522196552542,-0.46325952579966,4.027757291819));
#13086=CARTESIAN_POINT('Ctrl Pts',(14.3600910273042,-0.461383361236856,
3.9499475328577));
#13087=CARTESIAN_POINT('Ctrl Pts',(14.3679623993541,-0.441153180262727,
3.87724495265939));
#13088=CARTESIAN_POINT('Ctrl Pts',(14.3758337714041,-0.420922999288597,
3.80454237246108));
#13089=CARTESIAN_POINT('Ctrl Pts',(14.383705143454,-0.382338801903142,3.73694697102576));
#13090=CARTESIAN_POINT('Ctrl Pts',(14.391576515504,-0.330024073856894,3.68255860260764));
#13091=CARTESIAN_POINT('Ctrl Pts',(14.399447887554,-0.277709345810648,3.62817023418952));
#13092=CARTESIAN_POINT('Ctrl Pts',(14.4073192596039,-0.21166408710361,3.58698889878861));
#13093=CARTESIAN_POINT('Ctrl Pts',(14.4151906316539,-0.139802400742051,
3.56394929325792));
#13094=CARTESIAN_POINT('Ctrl Pts',(14.4230620037038,-0.0679407143804897,
3.54090968772722));
#13095=CARTESIAN_POINT('Ctrl Pts',(14.4309333757538,0.00973739963559066,
3.53601181206673));
#13096=CARTESIAN_POINT('Ctrl Pts',(14.4388047478037,0.0839238909224197,
3.54984257127538));
#13097=CARTESIAN_POINT('Ctrl Pts',(14.4466761198537,0.158110382209248,3.56367333048403));
#13098=CARTESIAN_POINT('Ctrl Pts',(14.4545474919037,0.228805250766822,3.59623272456181));
#13099=CARTESIAN_POINT('Ctrl Pts',(14.4624188639536,0.287537237904754,3.64361921078484));
#13100=CARTESIAN_POINT('Ctrl Pts',(14.4702902360036,0.346269225042686,3.69100569700788));
#13101=CARTESIAN_POINT('Ctrl Pts',(14.4781616080535,0.393038330760977,3.75321927537615));
#13102=CARTESIAN_POINT('Ctrl Pts',(14.4860329801035,0.422240284179214,3.8228049873169));
#13103=CARTESIAN_POINT('Ctrl Pts',(14.4939043521534,0.451442237597453,3.89239069925764));
#13104=CARTESIAN_POINT('Ctrl Pts',(14.5017757242034,0.463077038715637,3.96934854477086));
#13105=CARTESIAN_POINT('Ctrl Pts',(14.5096470962533,0.45575050699275,4.04445678215295));
#13106=CARTESIAN_POINT('Ctrl Pts',(14.5175184683033,0.448423975269863,4.11956501953505));
#13107=CARTESIAN_POINT('Ctrl Pts',(14.5253898403532,0.422136110705906,4.19282364878603));
#13108=CARTESIAN_POINT('Ctrl Pts',(14.5332612124032,0.380036948171907,4.2554541996672));
#13109=CARTESIAN_POINT('Ctrl Pts',(14.5411325844532,0.337937785637909,4.31808475054837));
#13110=CARTESIAN_POINT('Ctrl Pts',(14.5490039565031,0.28002732513387,4.37008722305972));
#13111=CARTESIAN_POINT('Ctrl Pts',(14.5568753285531,0.213244889156206,4.40523023992844));
#13112=CARTESIAN_POINT('Ctrl Pts',(14.5645849828737,0.147834501639678,4.43965124177167));
#13113=CARTESIAN_POINT('Ctrl Pts',(14.5722946371942,0.0739129441497101,
4.45789842831743));
#13114=CARTESIAN_POINT('Ctrl Pts',(14.5800042915148,-1.58578451148518E-6,
4.45791318879952));
#13115=CARTESIAN_POINT('Origin',(12.5,0.,4.));
#13116=CARTESIAN_POINT('',(14.8800042915148,-1.01702808208336E-5,4.45785711824254));
#13117=CARTESIAN_POINT('',(14.7699957084852,8.6346448269735E-6,4.45789857801605));
#13118=CARTESIAN_POINT('',(12.5,-5.60735153159594E-17,4.457875));
#13119=CARTESIAN_POINT('Ctrl Pts',(14.7699957084852,8.6346448269735E-6,
4.45789857801605));
#13120=CARTESIAN_POINT('Ctrl Pts',(14.7689821891192,0.00972641784825355,
4.45790700998655));
#13121=CARTESIAN_POINT('Ctrl Pts',(14.7679686697532,0.01944367562558,4.45760386164098));
#13122=CARTESIAN_POINT('Ctrl Pts',(14.7669551503872,0.0291408329004781,
4.45698549795522));
#13123=CARTESIAN_POINT('Ctrl Pts',(14.7590837783372,0.104452598317788,4.45218305332902));
#13124=CARTESIAN_POINT('Ctrl Pts',(14.7512124062873,0.178551969979598,4.4283678943965));
#13125=CARTESIAN_POINT('Ctrl Pts',(14.7433410342373,0.242559732875008,4.38839375563686));
#13126=CARTESIAN_POINT('Ctrl Pts',(14.7354696621874,0.30656749577042,4.34841961687722));
#13127=CARTESIAN_POINT('Ctrl Pts',(14.7275982901374,0.360483649899433,4.29228649829047));
#13128=CARTESIAN_POINT('Ctrl Pts',(14.7197269180875,0.397847504376097,4.22672074611392));
#13129=CARTESIAN_POINT('Ctrl Pts',(14.7118555460375,0.435211358852761,4.16115499393738));
#13130=CARTESIAN_POINT('Ctrl Pts',(14.7039841739875,0.456022913677073,4.08615660817103));
#13131=CARTESIAN_POINT('Ctrl Pts',(14.6961128019376,0.457788351878884,4.01071253147039));
#13132=CARTESIAN_POINT('Ctrl Pts',(14.6882414298876,0.459553790080695,3.93526845476975));
#13133=CARTESIAN_POINT('Ctrl Pts',(14.6803700578377,0.442273111660005,3.85937868713481));
#13134=CARTESIAN_POINT('Ctrl Pts',(14.6724986857877,0.408017034045316,3.79213698410258));
#13135=CARTESIAN_POINT('Ctrl Pts',(14.6646273137378,0.373760956430627,3.72489528107034));
#13136=CARTESIAN_POINT('Ctrl Pts',(14.6567559416878,0.32252947962194,3.6663016426408));
#13137=CARTESIAN_POINT('Ctrl Pts',(14.6488845696379,0.260461593653079,3.6233772554918));
#13138=CARTESIAN_POINT('Ctrl Pts',(14.6410131975879,0.198393707684219,3.5804528683428));
#13139=CARTESIAN_POINT('Ctrl Pts',(14.6331418255379,0.125489412555185,3.55319773247434));
#13140=CARTESIAN_POINT('Ctrl Pts',(14.625270453488,0.0504847191830214,3.54487778940425));
#13141=CARTESIAN_POINT('Ctrl Pts',(14.617399081438,-0.0245199741891427,
3.53655784633416));
#13142=CARTESIAN_POINT('Ctrl Pts',(14.6095277093881,-0.101625065804437,
3.54717309606245));
#13143=CARTESIAN_POINT('Ctrl Pts',(14.6016563373381,-0.171591169681571,
3.57545152934398));
#13144=CARTESIAN_POINT('Ctrl Pts',(14.5937849652882,-0.241557273558703,
3.6037299626255));
#13145=CARTESIAN_POINT('Ctrl Pts',(14.5859135932382,-0.304384389697674,
3.64967157946028));
#13146=CARTESIAN_POINT('Ctrl Pts',(14.5780422211883,-0.352544040227279,
3.70777126570269));
#13147=CARTESIAN_POINT('Ctrl Pts',(14.5701708491383,-0.400703690756885,
3.7658709519451));
#13148=CARTESIAN_POINT('Ctrl Pts',(14.5622994770883,-0.434195875677124,
3.83612870759516));
#13149=CARTESIAN_POINT('Ctrl Pts',(14.5544281050384,-0.449007277354457,
3.91012565253846));
#13150=CARTESIAN_POINT('Ctrl Pts',(14.5465567329884,-0.46381867903179,3.98412259748177));
#13151=CARTESIAN_POINT('Ctrl Pts',(14.5386853609385,-0.459949297466218,
4.06185873171832));
#13152=CARTESIAN_POINT('Ctrl Pts',(14.5308139888885,-0.437862794771992,
4.13401905238929));
#13153=CARTESIAN_POINT('Ctrl Pts',(14.5229426168386,-0.415776292077766,
4.20617937306026));
#13154=CARTESIAN_POINT('Ctrl Pts',(14.5150712447886,-0.375472668254887,
4.27276388016565));
#13155=CARTESIAN_POINT('Ctrl Pts',(14.5071998727387,-0.321781445311454,
4.32579385338299));
#13156=CARTESIAN_POINT('Ctrl Pts',(14.4993285006887,-0.26809022236802,4.37882382660034));
#13157=CARTESIAN_POINT('Ctrl Pts',(14.4914571286387,-0.201011400304033,
4.41829926592964));
#13158=CARTESIAN_POINT('Ctrl Pts',(14.4835857565888,-0.128582932452519,
4.43948988945229));
#13159=CARTESIAN_POINT('Ctrl Pts',(14.4790557405542,-0.0868999680795747,
4.45168520479633));
#13160=CARTESIAN_POINT('Ctrl Pts',(14.4745257245197,-0.0434451672832877,
4.45782447382869));
#13161=CARTESIAN_POINT('Ctrl Pts',(14.4699957084852,4.96934848862042E-6,
4.4578413260902));
#13162=CARTESIAN_POINT('Ctrl Pts',(14.5800042915148,-1.58578451148518E-6,
4.45791318879952));
#13163=CARTESIAN_POINT('Ctrl Pts',(14.5801660092442,-0.00155201715944126,
4.45791349841543));
#13164=CARTESIAN_POINT('Ctrl Pts',(14.5803277269736,-0.00310244544229786,
4.45790578589721));
#13165=CARTESIAN_POINT('Ctrl Pts',(14.5804894447029,-0.0046527920161852,
4.45789003224535));
#13166=CARTESIAN_POINT('Ctrl Pts',(14.5883608167529,-0.0801136257596197,
4.45712324646747));
#13167=CARTESIAN_POINT('Ctrl Pts',(14.5962321888029,-0.155380881795201,
4.43730611368561));
#13168=CARTESIAN_POINT('Ctrl Pts',(14.6041035608528,-0.22143539919095,4.4008132908088));
#13169=CARTESIAN_POINT('Ctrl Pts',(14.6119749329028,-0.287489916586699,
4.36432046793199));
#13170=CARTESIAN_POINT('Ctrl Pts',(14.6198463049527,-0.344331695342615,
4.31115195496024));
#13171=CARTESIAN_POINT('Ctrl Pts',(14.6277176770027,-0.38514947146564,4.24767885402976));
#13172=CARTESIAN_POINT('Ctrl Pts',(14.6355890490526,-0.425967247588666,
4.18420575309928));
#13173=CARTESIAN_POINT('Ctrl Pts',(14.6434604211026,-0.4507610210788,4.11042806421008));
#13174=CARTESIAN_POINT('Ctrl Pts',(14.6513317931525,-0.45655979174196,4.03518645571321));
#13175=CARTESIAN_POINT('Ctrl Pts',(14.6592031652025,-0.462358562405121,
3.95994484721634));
#13176=CARTESIAN_POINT('Ctrl Pts',(14.6670745372524,-0.449162330241309,
3.8832393191118));
#13177=CARTESIAN_POINT('Ctrl Pts',(14.6749459093024,-0.41855237967279,3.81426137832517));
#13178=CARTESIAN_POINT('Ctrl Pts',(14.6828172813524,-0.387942429104271,
3.74528343753854));
#13179=CARTESIAN_POINT('Ctrl Pts',(14.6906886534023,-0.339918760131043,
3.68403308406983));
#13180=CARTESIAN_POINT('Ctrl Pts',(14.6985600254523,-0.280235976103336,
3.63784985464301));
#13181=CARTESIAN_POINT('Ctrl Pts',(14.7064313975022,-0.220553192075631,
3.5916666252162));
#13182=CARTESIAN_POINT('Ctrl Pts',(14.7143027695522,-0.149211292993445,
3.5605505198313));
#13183=CARTESIAN_POINT('Ctrl Pts',(14.7221741416021,-0.0747590701011626,
3.54823013427646));
#13184=CARTESIAN_POINT('Ctrl Pts',(14.7300455136521,-0.000306847208877067,
3.53590974872161));
#13185=CARTESIAN_POINT('Ctrl Pts',(14.737916885702,0.0772556994935079,3.54238508299684));
#13186=CARTESIAN_POINT('Ctrl Pts',(14.745788257752,0.148634367597872,3.5668802073009));
#13187=CARTESIAN_POINT('Ctrl Pts',(14.753659629802,0.220013035702235,3.59137533160497));
#13188=CARTESIAN_POINT('Ctrl Pts',(14.7615310018519,0.285207825208577,3.63389024593787));
#13189=CARTESIAN_POINT('Ctrl Pts',(14.7694023739019,0.336406544142474,3.68933045342307));
#13190=CARTESIAN_POINT('Ctrl Pts',(14.7772737459518,0.387605263076371,3.74477066090827));
#13191=CARTESIAN_POINT('Ctrl Pts',(14.7851451180018,0.424807911437823,3.81313616154577));
#13192=CARTESIAN_POINT('Ctrl Pts',(14.7930164900517,0.443556551112275,3.88623481973509));
#13193=CARTESIAN_POINT('Ctrl Pts',(14.8008878621017,0.462305190786727,3.9593334779244));
#13194=CARTESIAN_POINT('Ctrl Pts',(14.8087592341516,0.462599821774179,4.03716529366552));
#13195=CARTESIAN_POINT('Ctrl Pts',(14.8166306062016,0.444405141642572,4.11040380200553));
#13196=CARTESIAN_POINT('Ctrl Pts',(14.8245019782516,0.426210461510966,4.18364231034555));
#13197=CARTESIAN_POINT('Ctrl Pts',(14.8323733503015,0.389526470260302,4.25228751128446));
#13198=CARTESIAN_POINT('Ctrl Pts',(14.8402447223515,0.338748948932789,4.3081137476731));
#13199=CARTESIAN_POINT('Ctrl Pts',(14.8481160944014,0.287971427605278,4.36393998406173));
#13200=CARTESIAN_POINT('Ctrl Pts',(14.8559874664514,0.22310037620092,4.40694725590009));
#13201=CARTESIAN_POINT('Ctrl Pts',(14.8638588385013,0.151909206873508,4.43198208217373));
#13202=CARTESIAN_POINT('Ctrl Pts',(14.8692406561725,0.103234351881841,4.44909890368578));
#13203=CARTESIAN_POINT('Ctrl Pts',(14.8746224738437,0.0516050086776526,
4.45781408155485));
#13204=CARTESIAN_POINT('Ctrl Pts',(14.8800042915148,-1.01702808208336E-5,
4.45785711824254));
#13205=CARTESIAN_POINT('Origin',(12.5,0.,4.));
#13206=CARTESIAN_POINT('',(15.1,-5.60735153159594E-17,4.457875));
#13207=CARTESIAN_POINT('',(15.0699957084852,-1.05870731373636E-5,4.45788944868556));
#13208=CARTESIAN_POINT('',(12.5,-5.60735153159594E-17,4.457875));
#13209=CARTESIAN_POINT('',(15.1,-0.269165465906718,4.37040446485999));
#13210=CARTESIAN_POINT('Origin',(15.1,0.,4.));
#13211=CARTESIAN_POINT('Ctrl Pts',(15.1,-0.269173508333955,4.37043259773194));
#13212=CARTESIAN_POINT('Ctrl Pts',(15.0991842588284,-0.262849866117432,
4.37503549456412));
#13213=CARTESIAN_POINT('Ctrl Pts',(15.0983685176569,-0.256407545646713,
4.37947450812006));
#13214=CARTESIAN_POINT('Ctrl Pts',(15.0975527764853,-0.249853611926923,
4.38374199825787));
#13215=CARTESIAN_POINT('Ctrl Pts',(15.0896814044354,-0.186612411779406,
4.42492050409441));
#13216=CARTESIAN_POINT('Ctrl Pts',(15.0818100323854,-0.112978907049287,
4.45012847221118));
#13217=CARTESIAN_POINT('Ctrl Pts',(15.0739386603355,-0.0377721395608013,
4.45635245505497));
#13218=CARTESIAN_POINT('Ctrl Pts',(15.072624343052,-0.0252145379490987,
4.45739170058566));
#13219=CARTESIAN_POINT('Ctrl Pts',(15.0713100257686,-0.0126130730861363,
4.45790166433459));
#13220=CARTESIAN_POINT('Ctrl Pts',(15.0699957084852,-1.05870731373636E-5,
4.45788944868556));
#13221=CARTESIAN_POINT('Origin',(11.8752146997001,0.,4.));
#13222=CARTESIAN_POINT('',(14.9247853002999,-1.38824472118437E-5,4.62497559137666));
#13223=CARTESIAN_POINT('',(15.0252146997001,-1.44513692928093E-5,4.62501972247551));
#13224=CARTESIAN_POINT('',(11.8752146997001,-1.68747709936658E-14,4.625));
#13225=CARTESIAN_POINT('',(15.1,-0.624993681275899,4.00281040303151));
#13226=CARTESIAN_POINT('Ctrl Pts',(15.0252146997001,-1.44513692928189E-5,
4.62501972247551));
#13227=CARTESIAN_POINT('Ctrl Pts',(15.0265290169835,-0.017216861979444,
4.62503639685311));
#13228=CARTESIAN_POINT('Ctrl Pts',(15.0357147063169,-0.137433797398843,
4.62017138475037));
#13229=CARTESIAN_POINT('Ctrl Pts',(15.0527717677003,-0.355236031271534,
4.54560815721762));
#13230=CARTESIAN_POINT('Ctrl Pts',(15.0763858838501,-0.571652475026301,
4.31158258982903));
#13231=CARTESIAN_POINT('Ctrl Pts',(15.09212862795,-0.624530364890795,4.10584538053252));
#13232=CARTESIAN_POINT('Ctrl Pts',(15.1,-0.624993681275899,4.00281040303152));
#13233=CARTESIAN_POINT('',(15.1,0.314930721058197,3.46014479632612));
#13234=CARTESIAN_POINT('Origin',(15.1,0.,4.));
#13235=CARTESIAN_POINT('Ctrl Pts',(14.9247853002999,-1.38824472118368E-5,
4.62497559137666));
#13236=CARTESIAN_POINT('Ctrl Pts',(14.9272748546787,-0.0326052931943186,
4.62500276606431));
#13237=CARTESIAN_POINT('Ctrl Pts',(14.9376357811074,-0.168225686180582,
4.61457389311938));
#13238=CARTESIAN_POINT('Ctrl Pts',(14.9558680795861,-0.394527586443172,
4.517903766532));
#13239=CARTESIAN_POINT('Ctrl Pts',(14.979482195736,-0.593077772790822,4.26857965265179));
#13240=CARTESIAN_POINT('Ctrl Pts',(15.0030963118859,-0.649493436571599,
3.95488773069898));
#13241=CARTESIAN_POINT('Ctrl Pts',(15.0267104280357,-0.550252000240565,
3.65200904506483));
#13242=CARTESIAN_POINT('Ctrl Pts',(15.0503245441856,-0.319142060764588,
3.43252503194012));
#13243=CARTESIAN_POINT('Ctrl Pts',(15.0739386603355,-0.0115409051696555,
3.34904846156061));
#13244=CARTESIAN_POINT('Ctrl Pts',(15.0904971456069,0.20608092381284,3.39989411918499));
#13245=CARTESIAN_POINT('Ctrl Pts',(15.0991842588284,0.305720220830039,3.45471854406458));
#13246=CARTESIAN_POINT('Ctrl Pts',(15.1,0.314937815442301,3.46010549098218));
#13247=CARTESIAN_POINT('Origin',(11.8752146997001,0.,4.));
#13248=CARTESIAN_POINT('',(14.6247853002999,-2.16459804047719E-6,4.62505212776347));
#13249=CARTESIAN_POINT('',(14.7252146997001,1.17863019661874E-5,4.62503218402409));
#13250=CARTESIAN_POINT('',(11.8752146997001,-1.68747709936658E-14,4.625));
#13251=CARTESIAN_POINT('Ctrl Pts',(14.7252146997001,1.17863019662174E-5,
4.62503218402409));
#13252=CARTESIAN_POINT('Ctrl Pts',(14.7320725523841,-0.0897427467603322,
4.62495430540108));
#13253=CARTESIAN_POINT('Ctrl Pts',(14.746801777118,-0.282587126126967,4.58296482291278));
#13254=CARTESIAN_POINT('Ctrl Pts',(14.7694023739019,-0.520130285395982,
4.39158760667368));
#13255=CARTESIAN_POINT('Ctrl Pts',(14.7930164900517,-0.64367318065081,4.09778141619902));
#13256=CARTESIAN_POINT('Ctrl Pts',(14.8166306062016,-0.612955311082805,
3.78054123783642));
#13257=CARTESIAN_POINT('Ctrl Pts',(14.8402447223515,-0.435338447621071,
3.51589585985611));
#13258=CARTESIAN_POINT('Ctrl Pts',(14.8638588385013,-0.153389665944836,
3.36726945127358));
#13259=CARTESIAN_POINT('Ctrl Pts',(14.8874729546512,0.165319955489652,3.37028123293502));
#13260=CARTESIAN_POINT('Ctrl Pts',(14.9110870708011,0.444409630539555,3.52420969451069));
#13261=CARTESIAN_POINT('Ctrl Pts',(14.9347011869509,0.616993161964042,3.79216419995926));
#13262=CARTESIAN_POINT('Ctrl Pts',(14.9583153031008,0.641710593195818,4.10992889087348));
#13263=CARTESIAN_POINT('Ctrl Pts',(14.9819294192507,0.512636325700993,4.40134645341462));
#13264=CARTESIAN_POINT('Ctrl Pts',(15.0042292181171,0.274729866520086,4.58571614948967));
#13265=CARTESIAN_POINT('Ctrl Pts',(15.0186576449336,0.0858074045169303,
4.62493653494651));
#13266=CARTESIAN_POINT('Ctrl Pts',(15.0252146997001,-1.44513692928189E-5,
4.62501972247551));
#13267=CARTESIAN_POINT('Ctrl Pts',(14.6247853002999,-2.16459804049194E-6,
4.62505212776347));
#13268=CARTESIAN_POINT('Ctrl Pts',(14.6249470180292,-0.00211850554115318,
4.62505255038961));
#13269=CARTESIAN_POINT('Ctrl Pts',(14.6329801078086,-0.107244412024774,
4.62452960748548));
#13270=CARTESIAN_POINT('Ctrl Pts',(14.6488845696379,-0.314835022974042,
4.56987302880665));
#13271=CARTESIAN_POINT('Ctrl Pts',(14.6724986857877,-0.547602339746838,
4.35214775046202));
#13272=CARTESIAN_POINT('Ctrl Pts',(14.6961128019376,-0.649132943719538,
4.05002781234082));
#13273=CARTESIAN_POINT('Ctrl Pts',(14.7197269180875,-0.595094318970103,
3.73591836064326));
#13274=CARTESIAN_POINT('Ctrl Pts',(14.7433410342373,-0.398437197867616,
3.48509791236843));
#13275=CARTESIAN_POINT('Ctrl Pts',(14.7669551503872,-0.1062918289807,3.35767733339665));
#13276=CARTESIAN_POINT('Ctrl Pts',(14.7905692665371,0.211327117384507,3.38419385377023));
#13277=CARTESIAN_POINT('Ctrl Pts',(14.8141833826869,0.478300047385911,3.5582926020622));
#13278=CARTESIAN_POINT('Ctrl Pts',(14.8377974988368,0.630645044771057,3.83824960712979));
#13279=CARTESIAN_POINT('Ctrl Pts',(14.8614116149867,0.631851559871185,4.15697121131127));
#13280=CARTESIAN_POINT('Ctrl Pts',(14.8850257311365,0.481630465478622,4.4380735902585));
#13281=CARTESIAN_POINT('Ctrl Pts',(14.9061502929076,0.243989509668873,4.59562135563586));
#13282=CARTESIAN_POINT('Ctrl Pts',(14.9194034826287,0.0704409072858971,
4.62491684623921));
#13283=CARTESIAN_POINT('Ctrl Pts',(14.9247853002999,-1.38824472118368E-5,
4.62497559137666));
#13284=CARTESIAN_POINT('Origin',(11.8752146997001,0.,4.));
#13285=CARTESIAN_POINT('',(14.3247853002999,1.51969053300144E-5,4.6249871875462));
#13286=CARTESIAN_POINT('',(14.4252146997001,6.78316748347314E-6,4.62495403506715));
#13287=CARTESIAN_POINT('',(11.8752146997001,-1.68747709936658E-14,4.625));
#13288=CARTESIAN_POINT('Ctrl Pts',(14.4252146997001,6.78316748347826E-6,
4.62495403506715));
#13289=CARTESIAN_POINT('Ctrl Pts',(14.4297447157347,-0.0593027126443913,
4.62493103170719));
#13290=CARTESIAN_POINT('Ctrl Pts',(14.4421461038192,-0.221686029527806,
4.60198961095629));
#13291=CARTESIAN_POINT('Ctrl Pts',(14.4624188639536,-0.457506203155893,
4.46321101183598));
#13292=CARTESIAN_POINT('Ctrl Pts',(14.4860329801035,-0.622549707754089,
4.19054718257559));
#13293=CARTESIAN_POINT('Ctrl Pts',(14.5096470962533,-0.63839484111024,3.87221739454711));
#13294=CARTESIAN_POINT('Ctrl Pts',(14.5332612124032,-0.501244206711231,
3.58451159745434));
#13295=CARTESIAN_POINT('Ctrl Pts',(14.5568753285531,-0.243966908844842,
3.39638048838484));
#13296=CARTESIAN_POINT('Ctrl Pts',(14.5804894447029,0.0717787570654544,
3.35291099727801));
#13297=CARTESIAN_POINT('Ctrl Pts',(14.6041035608528,0.370322144162233,3.46452089026927));
#13298=CARTESIAN_POINT('Ctrl Pts',(14.6277176770027,0.580115251486915,3.70446207957941));
#13299=CARTESIAN_POINT('Ctrl Pts',(14.6513317931525,0.650879700384091,4.0152309888134));
#13300=CARTESIAN_POINT('Ctrl Pts',(14.6749459093024,0.565656298155129,4.32234968564526));
#13301=CARTESIAN_POINT('Ctrl Pts',(14.6985600254523,0.344869426209941,4.55221503612336));
#13302=CARTESIAN_POINT('Ctrl Pts',(14.7153162889182,0.129554394067723,4.62141618582314));
#13303=CARTESIAN_POINT('Ctrl Pts',(14.7242011803341,0.0132765736394338,
4.62504369367533));
#13304=CARTESIAN_POINT('Ctrl Pts',(14.7252146997001,1.17863019662174E-5,
4.62503218402409));
#13305=CARTESIAN_POINT('Ctrl Pts',(14.3247853002999,1.51969053300109E-5,
4.6249871875462));
#13306=CARTESIAN_POINT('Ctrl Pts',(14.3304905534298,-0.0746697890657793,
4.62491698721088));
#13307=CARTESIAN_POINT('Ctrl Pts',(14.3440671786096,-0.252453835406249,
4.59302599116618));
#13308=CARTESIAN_POINT('Ctrl Pts',(14.3655151758395,-0.490432948250941,
4.42819608115853));
#13309=CARTESIAN_POINT('Ctrl Pts',(14.3891292919893,-0.634910852255616,
4.14409916841427));
#13310=CARTESIAN_POINT('Ctrl Pts',(14.4127434081392,-0.627227950688033,
3.82546788683648));
#13311=CARTESIAN_POINT('Ctrl Pts',(14.4363575242891,-0.469225504392149,
3.54866444115539));
#13312=CARTESIAN_POINT('Ctrl Pts',(14.4599716404389,-0.198769899531221,
3.38002670405092));
#13313=CARTESIAN_POINT('Ctrl Pts',(14.4835857565888,0.11932229545683,3.35996988316441));
#13314=CARTESIAN_POINT('Ctrl Pts',(14.5071998727387,0.408818071695872,3.49330073524378));
#13315=CARTESIAN_POINT('Ctrl Pts',(14.5308139888885,0.600337751131954,3.74806559342675));
#13316=CARTESIAN_POINT('Ctrl Pts',(14.5544281050384,0.647982309355475,4.06320828594604));
#13317=CARTESIAN_POINT('Ctrl Pts',(14.5780422211883,0.540333396317157,4.36320267272319));
#13318=CARTESIAN_POINT('Ctrl Pts',(14.6014946196088,0.304813865567294,4.57469465218781));
#13319=CARTESIAN_POINT('Ctrl Pts',(14.6170756459793,0.100891269655612,4.62503197968527));
#13320=CARTESIAN_POINT('Ctrl Pts',(14.6247853002999,-2.16459804049194E-6,
4.62505212776347));
#13321=CARTESIAN_POINT('Origin',(11.8752146997001,0.,4.));
#13322=CARTESIAN_POINT('',(14.0247853002999,-6.3966029390794E-6,4.62495348172753));
#13323=CARTESIAN_POINT('',(14.1252146997001,-1.50974863142078E-5,4.62498583382255));
#13324=CARTESIAN_POINT('',(11.8752146997001,-1.68747709936658E-14,4.625));
#13325=CARTESIAN_POINT('Ctrl Pts',(14.1252146997001,-1.50974863141889E-5,
4.62498583382255));
#13326=CARTESIAN_POINT('Ctrl Pts',(14.1274168790852,-0.0288430498503269,
4.62501265364587));
#13327=CARTESIAN_POINT('Ctrl Pts',(14.1374904305203,-0.160695812902997,
4.61605202430223));
#13328=CARTESIAN_POINT('Ctrl Pts',(14.1554353540053,-0.385112282251534,
4.52494275637564));
#13329=CARTESIAN_POINT('Ctrl Pts',(14.1790494701552,-0.588131968915973,
4.27924389796604));
#13330=CARTESIAN_POINT('Ctrl Pts',(14.2026635863051,-0.65020173504413,3.96662229549764));
#13331=CARTESIAN_POINT('Ctrl Pts',(14.2262777024549,-0.556446129094758,
3.66199989226673));
#13332=CARTESIAN_POINT('Ctrl Pts',(14.2498918186048,-0.329334334698108,
3.43838156778717));
#13333=CARTESIAN_POINT('Ctrl Pts',(14.2735059347547,-0.0232952743833569,
3.34935901020328));
#13334=CARTESIAN_POINT('Ctrl Pts',(14.2971200509045,0.28832666060365,3.41626709515619));
#13335=CARTESIAN_POINT('Ctrl Pts',(14.3207341670544,0.530849104237583,3.62307083431711));
#13336=CARTESIAN_POINT('Ctrl Pts',(14.3443482832043,0.646149864620809,3.92020827196535));
#13337=CARTESIAN_POINT('Ctrl Pts',(14.3679623993541,0.606596311879891,4.2364683526943));
#13338=CARTESIAN_POINT('Ctrl Pts',(14.391576515504,0.42166773027486,4.49605714656388));
#13339=CARTESIAN_POINT('Ctrl Pts',(14.4106606156193,0.190545343529355,4.60977018898031));
#13340=CARTESIAN_POINT('Ctrl Pts',(14.4218733436847,0.0437536792250838,
4.62497100242767));
#13341=CARTESIAN_POINT('Ctrl Pts',(14.4252146997001,6.78316748347826E-6,
4.62495403506715));
#13342=CARTESIAN_POINT('Ctrl Pts',(14.0247853002999,-6.39660293913491E-6,
4.62495348172753));
#13343=CARTESIAN_POINT('Ctrl Pts',(14.0281627167804,-0.0442255271350925,
4.62496963662755));
#13344=CARTESIAN_POINT('Ctrl Pts',(14.0394115053108,-0.191490205391595,
4.6095527480466));
#13345=CARTESIAN_POINT('Ctrl Pts',(14.0585316658912,-0.422790583021024,
4.49510047824495));
#13346=CARTESIAN_POINT('Ctrl Pts',(14.0821457820411,-0.60713052675338,4.23509335195577));
#13347=CARTESIAN_POINT('Ctrl Pts',(14.1057598981909,-0.645967413308333,
3.91874446730605));
#13348=CARTESIAN_POINT('Ctrl Pts',(14.1293740143408,-0.529993712466286,
3.62186903671368));
#13349=CARTESIAN_POINT('Ctrl Pts',(14.1529881304907,-0.287003328966194,
3.41561532377041));
#13350=CARTESIAN_POINT('Ctrl Pts',(14.1766022466405,0.0247694002478971,
3.34941346658496));
#13351=CARTESIAN_POINT('Ctrl Pts',(14.2002163627904,0.330605970264406,3.43912920108534));
#13352=CARTESIAN_POINT('Ctrl Pts',(14.2238304789403,0.557210518047066,3.66326152695696));
#13353=CARTESIAN_POINT('Ctrl Pts',(14.2474445950901,0.650275686248857,3.96809557204375));
#13354=CARTESIAN_POINT('Ctrl Pts',(14.27105871124,0.587497759452106,4.28057573538778));
#13355=CARTESIAN_POINT('Ctrl Pts',(14.2946728273899,0.383921904832036,4.52581397056352));
#13356=CARTESIAN_POINT('Ctrl Pts',(14.3125816904098,0.159750963363977,4.61623247111552));
#13357=CARTESIAN_POINT('Ctrl Pts',(14.3226191813798,0.0283709170587055,
4.62501384057475));
#13358=CARTESIAN_POINT('Ctrl Pts',(14.3247853002999,1.51969053300109E-5,
4.6249871875462));
#13359=CARTESIAN_POINT('Origin',(11.8752146997001,0.,4.));
#13360=CARTESIAN_POINT('',(13.7247853002999,-1.20831421157597E-5,4.62503091248755));
#13361=CARTESIAN_POINT('',(13.8252146997001,1.68461488569462E-6,4.62505238998457));
#13362=CARTESIAN_POINT('',(11.8752146997001,-1.68747709936658E-14,4.625));
#13363=CARTESIAN_POINT('Ctrl Pts',(13.8252146997001,1.68461488569581E-6,
4.62505238998457));
#13364=CARTESIAN_POINT('Ctrl Pts',(13.8329604144858,-0.101363538932993,
4.62503644193381));
#13365=CARTESIAN_POINT('Ctrl Pts',(13.8485775013214,-0.305753798836605,
4.57432856173903));
#13366=CARTESIAN_POINT('Ctrl Pts',(13.8720659602069,-0.541154937947787,
4.36197748624323));
#13367=CARTESIAN_POINT('Ctrl Pts',(13.8956800763568,-0.648123865072376,
4.06173996222779));
#13368=CARTESIAN_POINT('Ctrl Pts',(13.9192941925067,-0.599765396122921,
3.74670602647169));
#13369=CARTESIAN_POINT('Ctrl Pts',(13.9429083086565,-0.407668974822819,
3.49237575473668));
#13370=CARTESIAN_POINT('Ctrl Pts',(13.9665224248064,-0.117871845784803,
3.35970116712309));
#13371=CARTESIAN_POINT('Ctrl Pts',(13.9901365409563,0.200174091641329,3.38047865214521));
#13372=CARTESIAN_POINT('Ctrl Pts',(14.0137506571061,0.470246914526057,3.54972874087838));
#13373=CARTESIAN_POINT('Ctrl Pts',(14.037364773256,0.627621790796785,3.82688947135059));
#13374=CARTESIAN_POINT('Ctrl Pts',(14.0609788894059,0.634582735815489,4.14553734509456));
#13375=CARTESIAN_POINT('Ctrl Pts',(14.0845930055557,0.489461510650943,4.42930618095194));
#13376=CARTESIAN_POINT('Ctrl Pts',(14.1060049423205,0.251510284961593,4.59332024860173));
#13377=CARTESIAN_POINT('Ctrl Pts',(14.1195455070353,0.074198300926532,4.62491679006221));
#13378=CARTESIAN_POINT('Ctrl Pts',(14.1252146997001,-1.50974863141889E-5,
4.62498583382255));
#13379=CARTESIAN_POINT('Ctrl Pts',(13.7247853002999,-1.20831421156938E-5,
4.62503091248755));
#13380=CARTESIAN_POINT('Ctrl Pts',(13.7258348801309,-0.013748904810447,
4.62504304225186));
#13381=CARTESIAN_POINT('Ctrl Pts',(13.734755832012,-0.130498998332177,4.62127102305724));
#13382=CARTESIAN_POINT('Ctrl Pts',(13.7515481559429,-0.346119716157775,
4.55143222859795));
#13383=CARTESIAN_POINT('Ctrl Pts',(13.7751622720928,-0.566385203513325,
4.32106722332061));
#13384=CARTESIAN_POINT('Ctrl Pts',(13.7987763882427,-0.650912534047929,
4.01375622291695));
#13385=CARTESIAN_POINT('Ctrl Pts',(13.8223905043925,-0.57944414457563,3.70314844792952));
#13386=CARTESIAN_POINT('Ctrl Pts',(13.8460046205424,-0.369107932149097,
3.46368321387984));
#13387=CARTESIAN_POINT('Ctrl Pts',(13.8696187366923,-0.0703124342978696,
3.35275003110641));
#13388=CARTESIAN_POINT('Ctrl Pts',(13.8932328528421,0.245333927901481,3.3969348091043));
#13389=CARTESIAN_POINT('Ctrl Pts',(13.916846968992,0.502184306426786,3.58564835824111));
#13390=CARTESIAN_POINT('Ctrl Pts',(13.9404610851419,0.638682720042094,3.87366416276737));
#13391=CARTESIAN_POINT('Ctrl Pts',(13.9640752012917,0.62211637371287,4.19195723015293));
#13392=CARTESIAN_POINT('Ctrl Pts',(13.9876893174416,0.456455507660852,4.46424641105313));
#13393=CARTESIAN_POINT('Ctrl Pts',(14.007926017111,0.220741531225703,4.60224444133776));
#13394=CARTESIAN_POINT('Ctrl Pts',(14.0202913447304,0.058831122868106,4.62493198618401));
#13395=CARTESIAN_POINT('Ctrl Pts',(14.0247853002999,-6.39660293913491E-6,
4.62495348172753));
#13396=CARTESIAN_POINT('Origin',(11.8752146997001,0.,4.));
#13397=CARTESIAN_POINT('',(13.4247853002999,1.36962628664028E-5,4.62502243215823));
#13398=CARTESIAN_POINT('',(13.5252146997001,1.40828270379035E-5,4.62497680637469));
#13399=CARTESIAN_POINT('',(11.8752146997001,-1.68747709936658E-14,4.625));
#13400=CARTESIAN_POINT('Ctrl Pts',(13.5252146997001,1.4082827037902E-5,
4.62497680637469));
#13401=CARTESIAN_POINT('Ctrl Pts',(13.5306325778363,-0.0709123884867814,
4.62491668074428));
#13402=CARTESIAN_POINT('Ctrl Pts',(13.5439218280225,-0.244933372371362,
4.59533688876844));
#13403=CARTESIAN_POINT('Ctrl Pts',(13.5650824502587,-0.482621788093898,
4.43698120905743));
#13404=CARTESIAN_POINT('Ctrl Pts',(13.5886965664085,-0.632205603168059,
4.15553919999523));
#13405=CARTESIAN_POINT('Ctrl Pts',(13.6123106825584,-0.630276944445953,
3.83682113889318));
#13406=CARTESIAN_POINT('Ctrl Pts',(13.6359247987083,-0.477298028416376,
3.55721002779864));
#13407=CARTESIAN_POINT('Ctrl Pts',(13.6595389148582,-0.209931317243796,
3.38371661595291));
#13408=CARTESIAN_POINT('Ctrl Pts',(13.683153031008,0.107746895509167,3.35791980725116));
#13409=CARTESIAN_POINT('Ctrl Pts',(13.7067671471579,0.399602814690774,3.48600198647908));
#13410=CARTESIAN_POINT('Ctrl Pts',(13.7303812633077,0.59569113756138,3.73726736776131));
#13411=CARTESIAN_POINT('Ctrl Pts',(13.7539953794576,0.649017932507905,4.05149845333026));
#13412=CARTESIAN_POINT('Ctrl Pts',(13.7776094956075,0.546803061895555,4.35338757606046));
#13413=CARTESIAN_POINT('Ctrl Pts',(13.8012236117573,0.313543031018869,4.57058490613733));
#13414=CARTESIAN_POINT('Ctrl Pts',(13.8170920131216,0.106300066848774,4.6246481407235));
#13415=CARTESIAN_POINT('Ctrl Pts',(13.8250890424358,0.00164611344283092,
4.62505264870678));
#13416=CARTESIAN_POINT('Ctrl Pts',(13.8252146997001,1.68461488569581E-6,
4.62505238998457));
#13417=CARTESIAN_POINT('Ctrl Pts',(13.4247853002999,1.36962628664097E-5,
4.62502243215823));
#13418=CARTESIAN_POINT('Ctrl Pts',(13.4313784155315,-0.086279884022628,
4.62493973056585));
#13419=CARTESIAN_POINT('Ctrl Pts',(13.445842902813,-0.275670893367246,4.58538934244717));
#13420=CARTESIAN_POINT('Ctrl Pts',(13.4681787621445,-0.513544980480383,
4.40018484937968));
#13421=CARTESIAN_POINT('Ctrl Pts',(13.4917928782944,-0.64195771209056,4.10847422061066));
#13422=CARTESIAN_POINT('Ctrl Pts',(13.5154069944443,-0.616520809113462,
3.79076698974655));
#13423=CARTESIAN_POINT('Ctrl Pts',(13.5390211105941,-0.443330402422436,
3.52320390633144));
#13424=CARTESIAN_POINT('Ctrl Pts',(13.562635226744,-0.163892778617988,3.36990832590288));
#13425=CARTESIAN_POINT('Ctrl Pts',(13.5862493428939,0.154822890495328,3.36761860145296));
#13426=CARTESIAN_POINT('Ctrl Pts',(13.6098634590437,0.43643417612693,3.51688348138565));
#13427=CARTESIAN_POINT('Ctrl Pts',(13.6334775751936,0.613450973283793,3.78193059814177));
#13428=CARTESIAN_POINT('Ctrl Pts',(13.6570916913435,0.643449974253473,4.09923956510808));
#13429=CARTESIAN_POINT('Ctrl Pts',(13.6807058074933,0.519241709620395,4.39276507945606));
#13430=CARTESIAN_POINT('Ctrl Pts',(13.7032703438121,0.281645253009076,4.58329909926801));
#13431=CARTESIAN_POINT('Ctrl Pts',(13.717963508081,0.0892710189108511,4.62495207452848));
#13432=CARTESIAN_POINT('Ctrl Pts',(13.7247853002999,-1.20831421156938E-5,
4.62503091248755));
#13433=CARTESIAN_POINT('Origin',(11.8752146997001,0.,4.));
#13434=CARTESIAN_POINT('',(13.1247853002999,3.84888821539087E-6,4.62495078081483));
#13435=CARTESIAN_POINT('',(13.2252146997001,-9.32440196476731E-6,4.62495874418382));
#13436=CARTESIAN_POINT('',(11.8752146997001,-1.68747709936658E-14,4.625));
#13437=CARTESIAN_POINT('Ctrl Pts',(13.2252146997001,-9.32440196474427E-6,
4.62495874418382));
#13438=CARTESIAN_POINT('Ctrl Pts',(13.2283047411869,-0.040464997295585,
4.62498052751194));
#13439=CARTESIAN_POINT('Ctrl Pts',(13.2392661547237,-0.18396024524725,4.61125364372682));
#13440=CARTESIAN_POINT('Ctrl Pts',(13.2580989403104,-0.413782468289504,
4.50265339583901));
#13441=CARTESIAN_POINT('Ctrl Pts',(13.2817130564603,-0.602786876612853,
4.24601696851145));
#13442=CARTESIAN_POINT('Ctrl Pts',(13.3053271726101,-0.647329213752593,
3.9304208620728));
#13443=CARTESIAN_POINT('Ctrl Pts',(13.32894128876,-0.536734598538914,3.6314998804023));
#13444=CARTESIAN_POINT('Ctrl Pts',(13.3525554049099,-0.297507800394296,
3.42089251764738));
#13445=CARTESIAN_POINT('Ctrl Pts',(13.3761695210598,0.0130188131672444,
3.34907229440132));
#13446=CARTESIAN_POINT('Ctrl Pts',(13.3997836372096,0.320425377524893,3.43325142712992));
#13447=CARTESIAN_POINT('Ctrl Pts',(13.4233977533595,0.551039769569266,3.65325580067535));
#13448=CARTESIAN_POINT('Ctrl Pts',(13.4470118695093,0.649593644862141,3.95635983539258));
#13449=CARTESIAN_POINT('Ctrl Pts',(13.4706259856592,0.592467881122722,4.26992253935193));
#13450=CARTESIAN_POINT('Ctrl Pts',(13.4942401018091,0.393353065302923,4.5187964277335));
#13451=CARTESIAN_POINT('Ctrl Pts',(13.5124363398227,0.1672808180195,4.61476328251587));
#13452=CARTESIAN_POINT('Ctrl Pts',(13.5227612057864,0.0321332374692893,
4.62500403435298));
#13453=CARTESIAN_POINT('Ctrl Pts',(13.5252146997001,1.4082827037902E-5,
4.62497680637469));
#13454=CARTESIAN_POINT('Ctrl Pts',(13.1247853002999,3.84888821536311E-6,
4.62495078081483));
#13455=CARTESIAN_POINT('Ctrl Pts',(13.1290505788821,-0.0558403875021823,
4.6249385719914));
#13456=CARTESIAN_POINT('Ctrl Pts',(13.1411872295142,-0.214751600407627,
4.60383286368317));
#13457=CARTESIAN_POINT('Ctrl Pts',(13.1611952521963,-0.449738236712957,
4.47075670902068));
#13458=CARTESIAN_POINT('Ctrl Pts',(13.1848093683461,-0.619294173608025,
4.2008758003961));
#13459=CARTESIAN_POINT('Ctrl Pts',(13.208423484496,-0.64043195068177,3.88285360784221));
#13460=CARTESIAN_POINT('Ctrl Pts',(13.2320376006459,-0.508085752511173,
3.59290636366459));
#13461=CARTESIAN_POINT('Ctrl Pts',(13.2556517167957,-0.253973266794505,
3.40052194335125));
#13462=CARTESIAN_POINT('Ctrl Pts',(13.2792658329456,0.0610056803032868,
3.3518066124833));
#13463=CARTESIAN_POINT('Ctrl Pts',(13.3028799490955,0.361364191435218,3.45843533922715));
#13464=CARTESIAN_POINT('Ctrl Pts',(13.3264940652453,0.575119258511334,3.69485380694));
#13465=CARTESIAN_POINT('Ctrl Pts',(13.3501081813952,0.65104299168552,4.00440268404554));
#13466=CARTESIAN_POINT('Ctrl Pts',(13.3737222975451,0.570939739771795,4.31289642727099));
#13467=CARTESIAN_POINT('Ctrl Pts',(13.3973364136949,0.354006804717113,4.54640236352309));
#13468=CARTESIAN_POINT('Ctrl Pts',(13.4143574146132,0.136489422610972,4.62032507485564));
#13469=CARTESIAN_POINT('Ctrl Pts',(13.4235070434815,0.0167440814458925,
4.62503846613771));
#13470=CARTESIAN_POINT('Ctrl Pts',(13.4247853002999,1.36962628664097E-5,
4.62502243215823));
#13471=CARTESIAN_POINT('Origin',(11.8752146997001,0.,4.));
#13472=CARTESIAN_POINT('',(12.8247853002999,-1.55438223423121E-5,4.62499607812274));
#13473=CARTESIAN_POINT('',(12.9252146997001,-9.4222586321007E-6,4.62504029123831));
#13474=CARTESIAN_POINT('',(11.8752146997001,-1.68747709936658E-14,4.625));
#13475=CARTESIAN_POINT('Ctrl Pts',(12.9252146997001,-9.42225863212465E-6,
4.62504029123832));
#13476=CARTESIAN_POINT('Ctrl Pts',(12.9259769045375,-0.00998466834883174,
4.6250476064301));
#13477=CARTESIAN_POINT('Ctrl Pts',(12.9346104814248,-0.122971475467856,
4.62239759066569));
#13478=CARTESIAN_POINT('Ctrl Pts',(12.9511154303622,-0.336107011072318,
4.55759164674784));
#13479=CARTESIAN_POINT('Ctrl Pts',(12.974729546512,-0.56049590900091,4.33124115596169));
#13480=CARTESIAN_POINT('Ctrl Pts',(12.9983436626619,-0.650558060547343,
4.02550641626558));
#13481=CARTESIAN_POINT('Ctrl Pts',(13.0219577788117,-0.584709444123524,
3.71365888635357));
#13482=CARTESIAN_POINT('Ctrl Pts',(13.0455718949616,-0.378731139057797,
3.47043499764384));
#13483=CARTESIAN_POINT('Ctrl Pts',(13.0691860111115,-0.0819872800401352,
3.35412504823007));
#13484=CARTESIAN_POINT('Ctrl Pts',(13.0928001272613,0.234405401379786,3.39260352716186));
#13485=CARTESIAN_POINT('Ctrl Pts',(13.1164142434112,0.494621196584012,3.57664879910166));
#13486=CARTESIAN_POINT('Ctrl Pts',(13.1400283595611,0.636297578801308,3.86215313342763));
#13487=CARTESIAN_POINT('Ctrl Pts',(13.1636424757109,0.625480816776257,4.18069342892634));
#13488=CARTESIAN_POINT('Ctrl Pts',(13.1872565918608,0.464763222827219,4.45592928631477));
#13489=CARTESIAN_POINT('Ctrl Pts',(13.2077806665239,0.228267895462889,4.60018049807294));
#13490=CARTESIAN_POINT('Ctrl Pts',(13.220433369137,0.0625891701764018,4.62492503806923));
#13491=CARTESIAN_POINT('Ctrl Pts',(13.2252146997001,-9.32440196474427E-6,
4.62495874418382));
#13492=CARTESIAN_POINT('Ctrl Pts',(12.8247853002999,-1.55438223423052E-5,
4.62499607812274));
#13493=CARTESIAN_POINT('Ctrl Pts',(12.8267227422326,-0.0253767156259869,
4.62502109614712));
#13494=CARTESIAN_POINT('Ctrl Pts',(12.8365315562153,-0.153759343851268,
4.61735081595804));
#13495=CARTESIAN_POINT('Ctrl Pts',(12.854211742248,-0.376327535803878,4.5312757721487));
#13496=CARTESIAN_POINT('Ctrl Pts',(12.8778258583979,-0.583405888470749,
4.28898776831928));
#13497=CARTESIAN_POINT('Ctrl Pts',(12.9014399745477,-0.650666957548692,
3.97744183415536));
#13498=CARTESIAN_POINT('Ctrl Pts',(12.9250540906976,-0.561991161265395,
3.67130212143154));
#13499=CARTESIAN_POINT('Ctrl Pts',(12.9486682068475,-0.338630270727757,
3.44393714350224));
#13500=CARTESIAN_POINT('Ctrl Pts',(12.9722823229973,-0.0341142786054444,
3.34983650006563));
#13501=CARTESIAN_POINT('Ctrl Pts',(12.9958964391472,0.278577437919422,3.41155206540036));
#13502=CARTESIAN_POINT('Ctrl Pts',(13.0195105552971,0.524506132150044,3.61429327464512));
#13503=CARTESIAN_POINT('Ctrl Pts',(13.0431246714469,0.644733280558021,3.90947178565704));
#13504=CARTESIAN_POINT('Ctrl Pts',(13.0667387875968,0.61044561006836,4.22634601343335));
#13505=CARTESIAN_POINT('Ctrl Pts',(13.0903529037467,0.429860399609997,4.4889748434194));
#13506=CARTESIAN_POINT('Ctrl Pts',(13.1097017413144,0.197481915229314,4.60814700801091));
#13507=CARTESIAN_POINT('Ctrl Pts',(13.1211792068321,0.0472175377905832,
4.6249611028038));
#13508=CARTESIAN_POINT('Ctrl Pts',(13.1247853002999,3.84888821536311E-6,
4.62495078081483));
#13509=CARTESIAN_POINT('Origin',(11.8752146997001,0.,4.));
#13510=CARTESIAN_POINT('',(12.5247853002999,3.80998376854277E-6,4.62503871776264));
#13511=CARTESIAN_POINT('',(12.6252146997001,1.49489494596481E-5,4.6250110476872));
#13512=CARTESIAN_POINT('',(11.8752146997001,-1.68747709936658E-14,4.625));
#13513=CARTESIAN_POINT('',(12.5,0.310062960217711,4.54266560670548));
#13514=CARTESIAN_POINT('Ctrl Pts',(12.5,0.310062960217722,4.54266560670548));
#13515=CARTESIAN_POINT('Ctrl Pts',(12.50787137205,0.220600394030941,4.59378185169648));
#13516=CARTESIAN_POINT('Ctrl Pts',(12.5161331388166,0.113220056708515,4.6237347594226));
#13517=CARTESIAN_POINT('Ctrl Pts',(12.5243949055832,0.00511234815255113,
4.6250406321328));
#13518=CARTESIAN_POINT('Ctrl Pts',(12.5247853002999,3.80998376856706E-6,
4.62503871776264));
#13519=CARTESIAN_POINT('',(12.5,0.310062960217774,3.45733439329455));
#13520=CARTESIAN_POINT('Origin',(12.5,0.,4.));
#13521=CARTESIAN_POINT('Ctrl Pts',(12.5,0.310093463203755,3.45730861053195));
#13522=CARTESIAN_POINT('Ctrl Pts',(12.5008157411716,0.319367492808711,3.46259780682489));
#13523=CARTESIAN_POINT('Ctrl Pts',(12.5095028543931,0.416666480413896,3.52147574364868));
#13524=CARTESIAN_POINT('Ctrl Pts',(12.5260613396645,0.569511032758309,3.68451895614546));
#13525=CARTESIAN_POINT('Ctrl Pts',(12.5496754558144,0.651018771792273,3.99264764559437));
#13526=CARTESIAN_POINT('Ctrl Pts',(12.5732895719643,0.576495013506714,4.3025367374363));
#13527=CARTESIAN_POINT('Ctrl Pts',(12.5969036881141,0.363815091701307,4.53992168461618));
#13528=CARTESIAN_POINT('Ctrl Pts',(12.6142120640261,0.144017971622128,4.61907377583531));
#13529=CARTESIAN_POINT('Ctrl Pts',(12.6236490678881,0.0205077016108913,
4.62503160004571));
#13530=CARTESIAN_POINT('Ctrl Pts',(12.6252146997001,1.49489494596471E-5,
4.6250110476872));
#13531=CARTESIAN_POINT('Origin',(11.8752146997001,0.,4.));
#13532=CARTESIAN_POINT('Ctrl Pts',(12.6252146997001,1.49489494596471E-5,
4.6250110476872));
#13533=CARTESIAN_POINT('Ctrl Pts',(12.631520439938,-0.0825216819810338,
4.62492827098767));
#13534=CARTESIAN_POINT('Ctrl Pts',(12.6456975522259,-0.268159494659544,
4.5879440580038));
#13535=CARTESIAN_POINT('Ctrl Pts',(12.6677460365637,-0.506235857616531,
4.40939182910775));
#13536=CARTESIAN_POINT('Ctrl Pts',(12.6913601527136,-0.639894509617229,
4.12004729681268));
#13537=CARTESIAN_POINT('Ctrl Pts',(12.7149742688635,-0.620198095551099,
3.8019325752266));
#13538=CARTESIAN_POINT('Ctrl Pts',(12.7385883850133,-0.451866840211785,
3.53128609963859));
#13539=CARTESIAN_POINT('Ctrl Pts',(12.7622025011632,-0.17524257447904,3.37297016902465));
#13540=CARTESIAN_POINT('Ctrl Pts',(12.7858166173131,0.143379805101228,3.36492630429559));
#13541=CARTESIAN_POINT('Ctrl Pts',(12.809430733463,0.42764021116234,3.50908227080648));
#13542=CARTESIAN_POINT('Ctrl Pts',(12.8330448496128,0.609413666055986,3.77089008898231));
#13543=CARTESIAN_POINT('Ctrl Pts',(12.8566589657627,0.645136892431096,4.08760569204938));
#13544=CARTESIAN_POINT('Ctrl Pts',(12.8802730819125,0.526248572038732,4.38332598125533));
#13545=CARTESIAN_POINT('Ctrl Pts',(12.903124993225,0.289149347937084,4.5805996458561));
#13546=CARTESIAN_POINT('Ctrl Pts',(12.9181055324875,0.0930307802739178,
4.62497206165088));
#13547=CARTESIAN_POINT('Ctrl Pts',(12.9252146997001,-9.42225863212465E-6,
4.62504029123832));
#13548=CARTESIAN_POINT('Ctrl Pts',(12.5247853002999,3.80998376856706E-6,
4.62503871776264));
#13549=CARTESIAN_POINT('Ctrl Pts',(12.5322662776332,-0.0978890574527522,
4.62500203345524));
#13550=CARTESIAN_POINT('Ctrl Pts',(12.5476186270164,-0.298862923743373,
4.57698368148067));
#13551=CARTESIAN_POINT('Ctrl Pts',(12.5708423484496,-0.535054221536356,
4.37092866956447));
#13552=CARTESIAN_POINT('Ctrl Pts',(12.5944564645995,-0.647009713430093,
4.07251155115386));
#13553=CARTESIAN_POINT('Ctrl Pts',(12.6180705807493,-0.603894380709874,
3.75671714932517));
#13554=CARTESIAN_POINT('Ctrl Pts',(12.6416846968992,-0.416056506175611,
3.49922677321964));
#13555=CARTESIAN_POINT('Ctrl Pts',(12.6652988130491,-0.128505496873939,
3.36175035317655));
#13556=CARTESIAN_POINT('Ctrl Pts',(12.6889129291989,0.189841674427298,3.37723482234205));
#13557=CARTESIAN_POINT('Ctrl Pts',(12.7125270453488,0.462692468193658,3.54196933898577));
#13558=CARTESIAN_POINT('Ctrl Pts',(12.7361411614987,0.624655556881011,3.81647407445394));
#13559=CARTESIAN_POINT('Ctrl Pts',(12.7597552776485,0.636915702199809,4.13496208375113));
#13560=CARTESIAN_POINT('Ctrl Pts',(12.7833693937984,0.496534514683115,4.42110548633398));
#13561=CARTESIAN_POINT('Ctrl Pts',(12.8050460680155,0.258436396781676,4.5911312751119));
#13562=CARTESIAN_POINT('Ctrl Pts',(12.8188513701827,0.0776597756952025,
4.62491945378327));
#13563=CARTESIAN_POINT('Ctrl Pts',(12.8247853002999,-1.55438223423052E-5,
4.62499607812274));
#13564=CARTESIAN_POINT('Ctrl Pts',(12.5,-0.186196943290592,3.58169363627332));
#13565=CARTESIAN_POINT('Ctrl Pts',(12.50787137205,-0.117235947257613,3.55099764935784));
#13566=CARTESIAN_POINT('Ctrl Pts',(12.5236141161499,0.0360970477778841,
3.52440632583991));
#13567=CARTESIAN_POINT('Ctrl Pts',(12.5472282322997,0.257537368848111,3.59853698535937));
#13568=CARTESIAN_POINT('Ctrl Pts',(12.5708423484496,0.417223782598737,3.76887858727216));
#13569=CARTESIAN_POINT('Ctrl Pts',(12.5944564645995,0.476936352215019,3.99461366516243));
#13570=CARTESIAN_POINT('Ctrl Pts',(12.6180705807493,0.422340246895018,4.22163841384584));
#13571=CARTESIAN_POINT('Ctrl Pts',(12.6416846968992,0.266530936180377,4.39554662614981));
#13572=CARTESIAN_POINT('Ctrl Pts',(12.6652988130491,0.0468439715927196,
4.47465904879863));
#13573=CARTESIAN_POINT('Ctrl Pts',(12.6889129291989,-0.184068700558194,
4.44001626345752));
#13574=CARTESIAN_POINT('Ctrl Pts',(12.7125270453488,-0.37086838928987,4.29992045400434));
#13575=CARTESIAN_POINT('Ctrl Pts',(12.7361411614987,-0.468786717745582,
4.08794664964497));
#13576=CARTESIAN_POINT('Ctrl Pts',(12.7597552776485,-0.454357124800734,
3.85489580461101));
#13577=CARTESIAN_POINT('Ctrl Pts',(12.7833693937984,-0.331037647139153,
3.65662019659523));
#13578=CARTESIAN_POINT('Ctrl Pts',(12.8069835099483,-0.128382710063344,
3.54063794582746));
#13579=CARTESIAN_POINT('Ctrl Pts',(12.8305976260981,0.10504004521716,3.53474501052695));
#13580=CARTESIAN_POINT('Ctrl Pts',(12.854211742248,0.31328921869753,3.64035367159283));
#13581=CARTESIAN_POINT('Ctrl Pts',(12.8778258583979,0.446456451752615,3.83215407918844));
#13582=CARTESIAN_POINT('Ctrl Pts',(12.9014399745477,0.47262728739502,4.06417992999538));
#13583=CARTESIAN_POINT('Ctrl Pts',(12.9250540906976,0.385529703875575,4.28082461386765));
#13584=CARTESIAN_POINT('Ctrl Pts',(12.9486682068475,0.206037242841946,4.43016772408018));
#13585=CARTESIAN_POINT('Ctrl Pts',(12.9722823229973,-0.0228334776507366,
4.47641814468844));
#13586=CARTESIAN_POINT('Ctrl Pts',(12.9958964391472,-0.24623199631158,4.40849164040747));
#13587=CARTESIAN_POINT('Ctrl Pts',(13.0195105552971,-0.410619302934066,
4.24266727085754));
#13588=CARTESIAN_POINT('Ctrl Pts',(13.0431246714469,-0.476598835156983,
4.01868600055616));
#13589=CARTESIAN_POINT('Ctrl Pts',(13.0667387875968,-0.428358138764893,
3.79022650014263));
#13590=CARTESIAN_POINT('Ctrl Pts',(13.0903529037467,-0.277458432473742,
3.61204067927388));
#13591=CARTESIAN_POINT('Ctrl Pts',(13.1139670198965,-0.060063881357403,
3.52683201033335));
#13592=CARTESIAN_POINT('Ctrl Pts',(13.1375811360464,0.171725397050831,3.55502134399878));
#13593=CARTESIAN_POINT('Ctrl Pts',(13.1611952521963,0.362359488617447,3.68985291022187));
#13594=CARTESIAN_POINT('Ctrl Pts',(13.1848093683461,0.466151606229838,3.89901338554908));
#13595=CARTESIAN_POINT('Ctrl Pts',(13.208423484496,0.458227246370285,4.13237600603144));
#13596=CARTESIAN_POINT('Ctrl Pts',(13.2320376006459,0.34048553704322,4.3340137951542));
#13597=CARTESIAN_POINT('Ctrl Pts',(13.2556517167957,0.141144098528766,4.45560285308526));
#13598=CARTESIAN_POINT('Ctrl Pts',(13.2792658329456,-0.0920235057499227,
4.46800351566886));
#13599=CARTESIAN_POINT('Ctrl Pts',(13.3028799490955,-0.30313703626889,4.36824387779166));
#13600=CARTESIAN_POINT('Ctrl Pts',(13.3264940652453,-0.441601665806575,
4.18023203113149));
#13601=CARTESIAN_POINT('Ctrl Pts',(13.3501081813952,-0.47423338199515,3.94902632355453));
#13602=CARTESIAN_POINT('Ctrl Pts',(13.3737222975451,-0.393211766889608,
3.73003681238273));
#13603=CARTESIAN_POINT('Ctrl Pts',(13.3973364136949,-0.217954214568861,
3.57574585842847));
#13604=CARTESIAN_POINT('Ctrl Pts',(13.4209505298448,0.00953758252632317,
3.52313036287841));
#13605=CARTESIAN_POINT('Ctrl Pts',(13.4445646459947,0.234743631574736,3.58479999551538));
#13606=CARTESIAN_POINT('Ctrl Pts',(13.4681787621445,0.403691735186444,3.74597519957476));
#13607=CARTESIAN_POINT('Ctrl Pts',(13.4917928782944,0.475892304226004,3.96802921540861));
#13608=CARTESIAN_POINT('Ctrl Pts',(13.5154069944443,0.434041969710506,4.19774525232923));
#13609=CARTESIAN_POINT('Ctrl Pts',(13.5390211105941,0.288170455640921,4.38007026295756));
#13610=CARTESIAN_POINT('Ctrl Pts',(13.562635226744,0.0732368858249759,4.47130878927046));
#13611=CARTESIAN_POINT('Ctrl Pts',(13.5862493428939,-0.159248413505658,
4.44959488329479));
#13612=CARTESIAN_POINT('Ctrl Pts',(13.6098634590437,-0.353568721957589,
4.32013243375547));
#13613=CARTESIAN_POINT('Ctrl Pts',(13.6334775751936,-0.46315382488092,4.1139480179165));
#13614=CARTESIAN_POINT('Ctrl Pts',(13.6570916913435,-0.461740889501104,
3.88045516635315));
#13615=CARTESIAN_POINT('Ctrl Pts',(13.6807058074933,-0.349668535617837,
3.67561206636528));
#13616=CARTESIAN_POINT('Ctrl Pts',(13.7043199236432,-0.153795683012805,
3.5485107928471));
#13617=CARTESIAN_POINT('Ctrl Pts',(13.7279340397931,0.0789353756500159,
3.5296120507922));
#13618=CARTESIAN_POINT('Ctrl Pts',(13.7515481559429,0.292749022042461,3.62344505529457));
#13619=CARTESIAN_POINT('Ctrl Pts',(13.7751622720928,0.436403327377467,3.80752207362193));
#13620=CARTESIAN_POINT('Ctrl Pts',(13.7987763882427,0.475470537355291,4.03772776690975));
#13621=CARTESIAN_POINT('Ctrl Pts',(13.8223905043925,0.400587923144683,4.25889173822189));
#13622=CARTESIAN_POINT('Ctrl Pts',(13.8460046205424,0.229701624524423,4.41801050223621));
#13623=CARTESIAN_POINT('Ctrl Pts',(13.8696187366923,0.00376573255618155,
4.47695013947711));
#13624=CARTESIAN_POINT('Ctrl Pts',(13.8932328528421,-0.223072643433687,
4.42158535558109));
#13625=CARTESIAN_POINT('Ctrl Pts',(13.916846968992,-0.396450107540549,4.26518470642179));
#13626=CARTESIAN_POINT('Ctrl Pts',(13.9404610851419,-0.474815543552022,
4.04523069632808));
#13627=CARTESIAN_POINT('Ctrl Pts',(13.9640752012917,-0.439388129199652,
3.81443683499316));
#13628=CARTESIAN_POINT('Ctrl Pts',(13.9876893174416,-0.298658290955197,
3.62811447792009));
#13629=CARTESIAN_POINT('Ctrl Pts',(14.0113034335915,-0.0863529142219465,
3.53091707503438));
#13630=CARTESIAN_POINT('Ctrl Pts',(14.0349175497413,0.146647539536438,3.54613866056158));
#13631=CARTESIAN_POINT('Ctrl Pts',(14.0585316658912,0.344502889581789,3.6701312755675));
#13632=CARTESIAN_POINT('Ctrl Pts',(14.0821457820411,0.459795723937725,3.87317922671144));
#13633=CARTESIAN_POINT('Ctrl Pts',(14.1057598981909,0.464895312258427,4.10662065901627));
#13634=CARTESIAN_POINT('Ctrl Pts',(14.1293740143408,0.358579502702881,4.31450970816539));
#13635=CARTESIAN_POINT('Ctrl Pts',(14.1529881304907,0.166327619131383,4.44702431634421));
#13636=CARTESIAN_POINT('Ctrl Pts',(14.1766022466405,-0.0657858362277661,
4.47240643522367));
#13637=CARTESIAN_POINT('Ctrl Pts',(14.2002163627904,-0.282133257977474,
4.38457306332079));
#13638=CARTESIAN_POINT('Ctrl Pts',(14.2238304789403,-0.430865480427841,
4.20457407964992));
#13639=CARTESIAN_POINT('Ctrl Pts',(14.2474445950901,-0.476337791093329,
3.97554749368157));
#13640=CARTESIAN_POINT('Ctrl Pts',(14.27105871124,-0.407652434174819,3.75238112107461));
#13641=CARTESIAN_POINT('Ctrl Pts',(14.2946728273899,-0.241270333599833,
3.58855833656088));
#13642=CARTESIAN_POINT('Ctrl Pts',(14.3182869435397,-0.0170661180132474,
3.52334041087493));
#13643=CARTESIAN_POINT('Ctrl Pts',(14.3419010596896,0.211228111558234,3.57235727391142));
#13644=CARTESIAN_POINT('Ctrl Pts',(14.3655151758395,0.388900053764453,3.72386169322071));
#13645=CARTESIAN_POINT('Ctrl Pts',(14.3891292919893,0.473369390821204,3.94154458004181));
#13646=CARTESIAN_POINT('Ctrl Pts',(14.4127434081392,0.444392458083208,4.17323671518384));
#13647=CARTESIAN_POINT('Ctrl Pts',(14.4363575242891,0.308913779199362,4.3634114655727));
#13648=CARTESIAN_POINT('Ctrl Pts',(14.4599716404389,0.0994017626770733,
4.46649212840691));
#13649=CARTESIAN_POINT('Ctrl Pts',(14.4835857565888,-0.133932578240045,
4.45777470525894));
#13650=CARTESIAN_POINT('Ctrl Pts',(14.5071998727387,-0.335169044432007,
4.33934838727104));
#13651=CARTESIAN_POINT('Ctrl Pts',(14.5308139888885,-0.456079915900645,
4.13959486595487));
#13652=CARTESIAN_POINT('Ctrl Pts',(14.5544281050384,-0.467688060597361,
3.90638646324521));
#13653=CARTESIAN_POINT('Ctrl Pts',(14.5780422211883,-0.367211505836647,
3.69561319629505));
#13654=CARTESIAN_POINT('Ctrl Pts',(14.6016563373381,-0.178730157419731,
3.55778834579073));
#13655=CARTESIAN_POINT('Ctrl Pts',(14.625270453488,0.0525851174261518,3.52594259660587));
#13656=CARTESIAN_POINT('Ctrl Pts',(14.6488845696379,0.271298002813252,3.60770800421126));
#13657=CARTESIAN_POINT('Ctrl Pts',(14.6724986857877,0.424992433239313,3.78348891949988));
#13658=CARTESIAN_POINT('Ctrl Pts',(14.6961128019376,0.476834468501385,4.01115822240469));
#13659=CARTESIAN_POINT('Ctrl Pts',(14.7197269180875,0.414399804028447,4.23615337970372));
#13660=CARTESIAN_POINT('Ctrl Pts',(14.7433410342373,0.252651341641402,4.40455273546398));
#13661=CARTESIAN_POINT('Ctrl Pts',(14.7669551503872,0.0303532266559796,
4.47599821226155));
#13662=CARTESIAN_POINT('Ctrl Pts',(14.7905692665371,-0.199219250862459,
4.43336740322118));
#13663=CARTESIAN_POINT('Ctrl Pts',(14.8141833826869,-0.381047447081096,
4.28687708064914));
#13664=CARTESIAN_POINT('Ctrl Pts',(14.8377974988368,-0.471554972144783,
4.07163466550741));
#13665=CARTESIAN_POINT('Ctrl Pts',(14.8614116149867,-0.449051060899263,
3.83922451083896));
#13666=CARTESIAN_POINT('Ctrl Pts',(14.8850257311365,-0.318928946727196,
3.64534530693059));
#13667=CARTESIAN_POINT('Ctrl Pts',(14.9086398472864,-0.112373269271187,
3.53646160000302));
#13668=CARTESIAN_POINT('Ctrl Pts',(14.9322539634362,0.121113399391719,3.5386680312482));
#13669=CARTESIAN_POINT('Ctrl Pts',(14.9558680795861,0.325574495333277,3.65143602219853));
#13670=CARTESIAN_POINT('Ctrl Pts',(14.979482195736,0.452009190454857,3.84773949289016));
#13671=CARTESIAN_POINT('Ctrl Pts',(15.0030963118858,0.470117180575255,4.08053390545391));
#13672=CARTESIAN_POINT('Ctrl Pts',(15.0267104280357,0.375557372208547,4.29402641177155));
#13673=CARTESIAN_POINT('Ctrl Pts',(15.0503245441856,0.190994688421392,4.43705643304037));
#13674=CARTESIAN_POINT('Ctrl Pts',(15.0739386603355,-0.0393454023191647,
4.47533644032795));
#13675=CARTESIAN_POINT('Ctrl Pts',(15.0975527764853,-0.260245916509526,
4.39971253597763));
#13676=CARTESIAN_POINT('Ctrl Pts',(15.1211668926352,-0.418792603204267,
4.22826540530875));
#13677=CARTESIAN_POINT('Ctrl Pts',(15.1369096367351,-0.457530945318996,
4.07754232577813));
#13678=CARTESIAN_POINT('Ctrl Pts',(15.1447810087851,-0.457870370902723,
4.00205890126089));
#13679=CARTESIAN_POINT('Ctrl Pts',(12.4850729970717,-0.208850989443975,
3.53079950502365));
#13680=CARTESIAN_POINT('Ctrl Pts',(12.4929443691216,-0.131499707516366,
3.49636882573344));
#13681=CARTESIAN_POINT('Ctrl Pts',(12.5086871132215,0.0404888716816997,
3.46654221242176));
#13682=CARTESIAN_POINT('Ctrl Pts',(12.5323012293714,0.288871199237585,3.54969213591223));
#13683=CARTESIAN_POINT('Ctrl Pts',(12.5559153455212,0.467986199318594,3.74075871022993));
#13684=CARTESIAN_POINT('Ctrl Pts',(12.5795294616711,0.534963825407437,3.99395832530641));
#13685=CARTESIAN_POINT('Ctrl Pts',(12.603143577821,0.473725169098917,4.24860452170932));
#13686=CARTESIAN_POINT('Ctrl Pts',(12.6267576939708,0.298958988020687,4.4436716456386));
#13687=CARTESIAN_POINT('Ctrl Pts',(12.6503718101207,0.0525433427838623,
4.53240944903922));
#13688=CARTESIAN_POINT('Ctrl Pts',(12.6739859262706,-0.206463809544117,
4.49355177571912));
#13689=CARTESIAN_POINT('Ctrl Pts',(12.6976000424205,-0.41599087873209,4.33641091237214));
#13690=CARTESIAN_POINT('Ctrl Pts',(12.7212141585703,-0.525822648369464,
4.09864686536754));
#13691=CARTESIAN_POINT('Ctrl Pts',(12.7448282747202,-0.509637448384189,
3.8372413948162));
#13692=CARTESIAN_POINT('Ctrl Pts',(12.76844239087,-0.37131404483003,3.61484216427635));
#13693=CARTESIAN_POINT('Ctrl Pts',(12.7920565070199,-0.144002664868576,
3.48474868689319));
#13694=CARTESIAN_POINT('Ctrl Pts',(12.8156706231698,0.117819965178516,3.47813877511649));
#13695=CARTESIAN_POINT('Ctrl Pts',(12.8392847393197,0.351406216185799,3.59659653799738));
#13696=CARTESIAN_POINT('Ctrl Pts',(12.8628988554695,0.500775523187073,3.81173274911973));
#13697=CARTESIAN_POINT('Ctrl Pts',(12.8865129716194,0.530130489073712,4.07198851734671));
#13698=CARTESIAN_POINT('Ctrl Pts',(12.9101270877692,0.432435993263294,4.31499173633021));
#13699=CARTESIAN_POINT('Ctrl Pts',(12.9337412039191,0.231105201134755,4.48250499290311));
#13700=CARTESIAN_POINT('Ctrl Pts',(12.957355320069,-0.0256115611541523,
4.53438256906268));
#13701=CARTESIAN_POINT('Ctrl Pts',(12.9809694362189,-0.276190334565159,
4.45819164252092));
#13702=CARTESIAN_POINT('Ctrl Pts',(13.0045835523687,-0.460578171623014,
4.27219189922559));
#13703=CARTESIAN_POINT('Ctrl Pts',(13.0281976685186,-0.534585243620437,
4.0209594724593));
#13704=CARTESIAN_POINT('Ctrl Pts',(13.0518117846684,-0.480475240551103,
3.76470396221295));
#13705=CARTESIAN_POINT('Ctrl Pts',(13.0754259008183,-0.311216001335094,
3.5648387853972));
#13706=CARTESIAN_POINT('Ctrl Pts',(13.0990400169682,-0.0673716809183137,
3.46926302296559));
#13707=CARTESIAN_POINT('Ctrl Pts',(13.122654133118,0.19261873182715,3.50088207171981));
#13708=CARTESIAN_POINT('Ctrl Pts',(13.1462682492679,0.406446724606302,3.65211820651514));
#13709=CARTESIAN_POINT('Ctrl Pts',(13.1698823654178,0.522866930420328,3.88672663484193));
#13710=CARTESIAN_POINT('Ctrl Pts',(13.1934964815676,0.513978436505609,4.14848181366307));
#13711=CARTESIAN_POINT('Ctrl Pts',(13.2171105977175,0.381911432304553,4.37465229220773));
#13712=CARTESIAN_POINT('Ctrl Pts',(13.2407247138674,0.158316694737061,4.51103474084347));
#13713=CARTESIAN_POINT('Ctrl Pts',(13.2643388300172,-0.103219740820234,
4.52494415635039));
#13714=CARTESIAN_POINT('Ctrl Pts',(13.2879529461671,-0.340018846942428,
4.41304705047411));
#13715=CARTESIAN_POINT('Ctrl Pts',(13.311567062317,-0.495330069408668,4.20216034359148));
#13716=CARTESIAN_POINT('Ctrl Pts',(13.3351811784669,-0.531931992580964,
3.94282450306062));
#13717=CARTESIAN_POINT('Ctrl Pts',(13.3587952946167,-0.44105271077271,3.69719116838925));
#13718=CARTESIAN_POINT('Ctrl Pts',(13.3824094107666,-0.244472076510672,
3.5241280781681));
#13719=CARTESIAN_POINT('Ctrl Pts',(13.4060235269164,0.0106979927399635,
3.46511100671938));
#13720=CARTESIAN_POINT('Ctrl Pts',(13.4296376430663,0.263304213558122,3.53428380605355));
#13721=CARTESIAN_POINT('Ctrl Pts',(13.4532517592162,0.452807746647384,3.71506873327496));
#13722=CARTESIAN_POINT('Ctrl Pts',(13.476865875366,0.533792751104717,3.96413942206993));
#13723=CARTESIAN_POINT('Ctrl Pts',(13.5004799915159,0.486850606847911,4.22180434800346));
#13724=CARTESIAN_POINT('Ctrl Pts',(13.5240941076658,0.323231325528255,4.42631231788287));
#13725=CARTESIAN_POINT('Ctrl Pts',(13.5477082238157,0.0821474069231642,
4.52865157307741));
#13726=CARTESIAN_POINT('Ctrl Pts',(13.5713223399655,-0.178623709606947,
4.50429579866153));
#13727=CARTESIAN_POINT('Ctrl Pts',(13.5949364561154,-0.396586410669692,
4.35908202552279));
#13728=CARTESIAN_POINT('Ctrl Pts',(13.6185505722652,-0.519504417643299,
4.12781174527607));
#13729=CARTESIAN_POINT('Ctrl Pts',(13.6421646884151,-0.517919574482721,
3.86591049053316));
#13730=CARTESIAN_POINT('Ctrl Pts',(13.665778804565,-0.392211699884016,3.6361447201764));
#13731=CARTESIAN_POINT('Ctrl Pts',(13.6893929207148,-0.172507561089802,
3.49357940054904));
#13732=CARTESIAN_POINT('Ctrl Pts',(13.7130070368647,0.0885392156030666,
3.47238130294519));
#13733=CARTESIAN_POINT('Ctrl Pts',(13.7366211530146,0.328366952925232,3.57763069902274));
#13734=CARTESIAN_POINT('Ctrl Pts',(13.7602352691644,0.489499264105438,3.78410383833506));
#13735=CARTESIAN_POINT('Ctrl Pts',(13.7838493853143,0.533319669072828,4.04231799571659));
#13736=CARTESIAN_POINT('Ctrl Pts',(13.8074635014642,0.449326302728307,4.29039035083475));
#13737=CARTESIAN_POINT('Ctrl Pts',(13.831077617614,0.257648760022572,4.46886863686992));
#13738=CARTESIAN_POINT('Ctrl Pts',(13.8546917337639,0.00422389839726028,
4.53497929012603));
#13739=CARTESIAN_POINT('Ctrl Pts',(13.8783058499138,-0.25021324988294,4.47287843233165));
#13740=CARTESIAN_POINT('Ctrl Pts',(13.9019199660636,-0.444685051009628,
4.29744896636227));
#13741=CARTESIAN_POINT('Ctrl Pts',(13.9255340822135,-0.532584984058807,
4.05073378496132));
#13742=CARTESIAN_POINT('Ctrl Pts',(13.9491481983634,-0.492847218174075,
3.79185989881933));
#13743=CARTESIAN_POINT('Ctrl Pts',(13.9727623145132,-0.334995185577738,
3.58286823685896));
#13744=CARTESIAN_POINT('Ctrl Pts',(13.9963764306631,-0.0968592247428986,
3.47384510573062));
#13745=CARTESIAN_POINT('Ctrl Pts',(14.019990546813,0.164489723571401,3.49091865775613));
#13746=CARTESIAN_POINT('Ctrl Pts',(14.0436046629628,0.386417564563212,3.62999709733779));
#13747=CARTESIAN_POINT('Ctrl Pts',(14.0672187791127,0.515737746224078,3.85774930825782));
#13748=CARTESIAN_POINT('Ctrl Pts',(14.0908328952626,0.521457786777448,4.11959288770904));
#13749=CARTESIAN_POINT('Ctrl Pts',(14.1144470114124,0.402206838685568,4.35277519909424));
#13750=CARTESIAN_POINT('Ctrl Pts',(14.1380611275623,0.186564221804844,4.50141247822903));
#13751=CARTESIAN_POINT('Ctrl Pts',(14.1616752437122,-0.0737898095680628,
4.52988276645436));
#13752=CARTESIAN_POINT('Ctrl Pts',(14.185289359862,-0.316459599402161,4.43136296100575));
#13753=CARTESIAN_POINT('Ctrl Pts',(14.2089034760119,-0.483287643257218,
4.22946401908862));
#13754=CARTESIAN_POINT('Ctrl Pts',(14.2325175921618,-0.53429243907693,3.97257242762026));
#13755=CARTESIAN_POINT('Ctrl Pts',(14.2561317083116,-0.457250332481466,
3.72225404480531));
#13756=CARTESIAN_POINT('Ctrl Pts',(14.2797458244615,-0.270625000632592,
3.53849941363631));
#13757=CARTESIAN_POINT('Ctrl Pts',(14.3033599406114,-0.0191425034699505,
3.46534661065105));
#13758=CARTESIAN_POINT('Ctrl Pts',(14.3269740567612,0.236927627906706,3.52032721432634));
#13759=CARTESIAN_POINT('Ctrl Pts',(14.3505881729111,0.436216403922163,3.69026474025285));
#13760=CARTESIAN_POINT('Ctrl Pts',(14.374202289061,0.530962882087739,3.93443247734966));
#13761=CARTESIAN_POINT('Ctrl Pts',(14.3978164052108,0.498460409348769,4.19431392768733));
#13762=CARTESIAN_POINT('Ctrl Pts',(14.4214305213607,0.346498429557861,4.40762669256976));
#13763=CARTESIAN_POINT('Ctrl Pts',(14.4450446375106,0.111495689030631,4.52324888295055));
#13764=CARTESIAN_POINT('Ctrl Pts',(14.4686587536604,-0.150227769531968,
4.51347083601981));
#13765=CARTESIAN_POINT('Ctrl Pts',(14.4922728698103,-0.375948097339969,
4.38063592879268));
#13766=CARTESIAN_POINT('Ctrl Pts',(14.5158869859602,-0.51156984651846,4.15657897149511));
#13767=CARTESIAN_POINT('Ctrl Pts',(14.53950110211,-0.52459032076832,3.89499677367918));
#13768=CARTESIAN_POINT('Ctrl Pts',(14.5631152182599,-0.411889072794842,
3.65857933001481));
#13769=CARTESIAN_POINT('Ctrl Pts',(14.5867293344098,-0.200475741228102,
3.50398572665543));
#13770=CARTESIAN_POINT('Ctrl Pts',(14.6103434505596,0.0589829973059192,
3.46826539682992));
#13771=CARTESIAN_POINT('Ctrl Pts',(14.6339575667095,0.304306049929579,3.5599789662306));
#13772=CARTESIAN_POINT('Ctrl Pts',(14.6575716828594,0.476700039321847,3.75714663952638));
#13773=CARTESIAN_POINT('Ctrl Pts',(14.6811857990092,0.53484954579562,4.0125158112076));
#13774=CARTESIAN_POINT('Ctrl Pts',(14.7047999151591,0.464818635404008,4.26488548168423));
#13775=CARTESIAN_POINT('Ctrl Pts',(14.728414031309,0.283390703164248,4.45377350235044));
#13776=CARTESIAN_POINT('Ctrl Pts',(14.7520281474588,0.0340462163765225,
4.5339115446661));
#13777=CARTESIAN_POINT('Ctrl Pts',(14.7756422636087,-0.223457683695575,
4.48609396779546));
#13778=CARTESIAN_POINT('Ctrl Pts',(14.7992563797586,-0.427408393186059,
4.32178058932398));
#13779=CARTESIAN_POINT('Ctrl Pts',(14.8228704959084,-0.528927708313459,
4.08035024907128));
#13780=CARTESIAN_POINT('Ctrl Pts',(14.8464846120583,-0.503685810960444,
3.81966341983811));
#13781=CARTESIAN_POINT('Ctrl Pts',(14.8700987282082,-0.357732113691821,
3.6021954912391));
#13782=CARTESIAN_POINT('Ctrl Pts',(14.893712844358,-0.126045401495737,3.48006421709321));
#13783=CARTESIAN_POINT('Ctrl Pts',(14.9173269605079,0.13584891809103,3.48253909847714));
#13784=CARTESIAN_POINT('Ctrl Pts',(14.9409410766578,0.365186207068703,3.60902724630258));
#13785=CARTESIAN_POINT('Ctrl Pts',(14.9645551928076,0.507003847624586,3.82921439524653));
#13786=CARTESIAN_POINT('Ctrl Pts',(14.9881693089575,0.52731498478211,4.0903322339271));
#13787=CARTESIAN_POINT('Ctrl Pts',(15.0117834251074,0.421250356706029,4.32979975898591));
#13788=CARTESIAN_POINT('Ctrl Pts',(15.0353975412572,0.214232462415332,4.49023183125449));
#13789=CARTESIAN_POINT('Ctrl Pts',(15.0590116574071,-0.0441324441701724,
4.53316925684615));
#13790=CARTESIAN_POINT('Ctrl Pts',(15.082625773557,-0.291909288096862,4.4483444097243));
#13791=CARTESIAN_POINT('Ctrl Pts',(15.1062398897068,-0.469745893811612,
4.25603780014884));
#13792=CARTESIAN_POINT('Ctrl Pts',(15.1219826338067,-0.513197418509596,
4.08697667736293));
#13793=CARTESIAN_POINT('Ctrl Pts',(15.1298540058567,-0.513578141027115,
4.0023094018511));
#13794=CARTESIAN_POINT('Ctrl Pts',(12.4701459941433,-0.231505035597357,
3.47990537377399));
#13795=CARTESIAN_POINT('Ctrl Pts',(12.4780173661933,-0.145763467775118,
3.44174000210903));
#13796=CARTESIAN_POINT('Ctrl Pts',(12.4937601102932,0.0448806955855158,
3.40867809900361));
#13797=CARTESIAN_POINT('Ctrl Pts',(12.517374226443,0.320205029627059,3.5008472864651));
#13798=CARTESIAN_POINT('Ctrl Pts',(12.5409883425929,0.518748616038451,3.71263883318769));
#13799=CARTESIAN_POINT('Ctrl Pts',(12.5646024587428,0.592991298599855,3.99330298545039));
#13800=CARTESIAN_POINT('Ctrl Pts',(12.5882165748926,0.525110091302815,4.27557062957281));
#13801=CARTESIAN_POINT('Ctrl Pts',(12.6118306910425,0.331387039860997,4.49179666512739));
#13802=CARTESIAN_POINT('Ctrl Pts',(12.6354448071924,0.0582427139750047,
4.5901598492798));
#13803=CARTESIAN_POINT('Ctrl Pts',(12.6590589233422,-0.22885891853004,4.54708728798072));
#13804=CARTESIAN_POINT('Ctrl Pts',(12.6826730394921,-0.461113368174311,
4.37290137073994));
#13805=CARTESIAN_POINT('Ctrl Pts',(12.706287155642,-0.582858578993347,4.10934708109011));
#13806=CARTESIAN_POINT('Ctrl Pts',(12.7299012717918,-0.564917771967644,
3.8195869850214));
#13807=CARTESIAN_POINT('Ctrl Pts',(12.7535153879417,-0.411590442520908,
3.57306413195747));
#13808=CARTESIAN_POINT('Ctrl Pts',(12.7771295040916,-0.159622619673808,
3.42885942795892));
#13809=CARTESIAN_POINT('Ctrl Pts',(12.8007436202414,0.130599885139872,3.42153253970604));
#13810=CARTESIAN_POINT('Ctrl Pts',(12.8243577363913,0.38952321367407,3.55283940440193));
#13811=CARTESIAN_POINT('Ctrl Pts',(12.8479718525412,0.555094594621529,3.79131141905102));
#13812=CARTESIAN_POINT('Ctrl Pts',(12.871585968691,0.587633690752404,4.07979710469805));
#13813=CARTESIAN_POINT('Ctrl Pts',(12.8952000848409,0.479342282651013,4.34915885879276));
#13814=CARTESIAN_POINT('Ctrl Pts',(12.9188142009908,0.256173159427565,4.53484226172604));
#13815=CARTESIAN_POINT('Ctrl Pts',(12.9424283171406,-0.0283896446575681,
4.59234699343691));
#13816=CARTESIAN_POINT('Ctrl Pts',(12.9660424332905,-0.306148672818738,
4.50789164463438));
#13817=CARTESIAN_POINT('Ctrl Pts',(12.9896565494404,-0.510537040311962,
4.30171652759364));
#13818=CARTESIAN_POINT('Ctrl Pts',(13.0132706655902,-0.59257165208389,4.02323294436244));
#13819=CARTESIAN_POINT('Ctrl Pts',(13.0368847817401,-0.532592342337314,
3.73918142428326));
#13820=CARTESIAN_POINT('Ctrl Pts',(13.06049889789,-0.344973570196446,3.51763689152052));
#13821=CARTESIAN_POINT('Ctrl Pts',(13.0841130140398,-0.0746794804792245,
3.41169403559782));
#13822=CARTESIAN_POINT('Ctrl Pts',(13.1077271301897,0.213512066603468,3.44674279944083));
#13823=CARTESIAN_POINT('Ctrl Pts',(13.1313412463396,0.450533960595157,3.6143835028084));
#13824=CARTESIAN_POINT('Ctrl Pts',(13.1549553624894,0.579582254610818,3.87443988413478));
#13825=CARTESIAN_POINT('Ctrl Pts',(13.1785694786393,0.569729626640933,4.1645876212947));
#13826=CARTESIAN_POINT('Ctrl Pts',(13.2021835947892,0.423337327565886,4.41529078926125));
#13827=CARTESIAN_POINT('Ctrl Pts',(13.225797710939,0.175489290945357,4.56646662860168));
#13828=CARTESIAN_POINT('Ctrl Pts',(13.2494118270889,-0.114415975890545,
4.58188479703192));
#13829=CARTESIAN_POINT('Ctrl Pts',(13.2730259432388,-0.376900657615966,
4.45785022315656));
#13830=CARTESIAN_POINT('Ctrl Pts',(13.2966400593886,-0.54905847301076,4.22408865605146));
#13831=CARTESIAN_POINT('Ctrl Pts',(13.3202541755385,-0.589630603166779,
3.93662268256671));
#13832=CARTESIAN_POINT('Ctrl Pts',(13.3438682916884,-0.488893654655812,
3.66434552439578));
#13833=CARTESIAN_POINT('Ctrl Pts',(13.3674824078382,-0.270989938452484,
3.47251029790774));
#13834=CARTESIAN_POINT('Ctrl Pts',(13.3910965239881,0.0118584029536041,
3.40709165056035));
#13835=CARTESIAN_POINT('Ctrl Pts',(13.414710640138,0.291864795541507,3.48376761659174));
#13836=CARTESIAN_POINT('Ctrl Pts',(13.4383247562878,0.501923758108325,3.68416226697515));
#13837=CARTESIAN_POINT('Ctrl Pts',(13.4619388724377,0.591693197983429,3.96024962873126));
#13838=CARTESIAN_POINT('Ctrl Pts',(13.4855529885876,0.539659243985316,4.2458634436777));
#13839=CARTESIAN_POINT('Ctrl Pts',(13.5091671047374,0.358292195415589,4.47255437280819));
#13840=CARTESIAN_POINT('Ctrl Pts',(13.5327812208873,0.0910579280213527,
4.58599435688436));
#13841=CARTESIAN_POINT('Ctrl Pts',(13.5563953370372,-0.197999005708236,
4.55899671402827));
#13842=CARTESIAN_POINT('Ctrl Pts',(13.580009453187,-0.439604099381795,4.39803161729011));
#13843=CARTESIAN_POINT('Ctrl Pts',(13.6036235693369,-0.575855010405679,
4.14167547263565));
#13844=CARTESIAN_POINT('Ctrl Pts',(13.6272376854868,-0.574098259464336,
3.85136581471317));
#13845=CARTESIAN_POINT('Ctrl Pts',(13.6508518016366,-0.434754864150196,
3.59667737398752));
#13846=CARTESIAN_POINT('Ctrl Pts',(13.6744659177865,-0.191219439166798,
3.43864800825098));
#13847=CARTESIAN_POINT('Ctrl Pts',(13.6980800339364,0.0981430555561168,
3.41515055509818));
#13848=CARTESIAN_POINT('Ctrl Pts',(13.7216941500862,0.363984883808003,3.53181634275091));
#13849=CARTESIAN_POINT('Ctrl Pts',(13.7453082662361,0.54259520083341,3.76068560304818));
#13850=CARTESIAN_POINT('Ctrl Pts',(13.768922382386,0.591168800790367,4.04690822452342));
#13851=CARTESIAN_POINT('Ctrl Pts',(13.7925364985358,0.498064682311931,4.32188896344761));
#13852=CARTESIAN_POINT('Ctrl Pts',(13.8161506146857,0.28559589552072,4.51972677150362));
#13853=CARTESIAN_POINT('Ctrl Pts',(13.8397647308356,0.00468206423833927,
4.59300844077494));
#13854=CARTESIAN_POINT('Ctrl Pts',(13.8633788469854,-0.277353856332193,
4.52417150908221));
#13855=CARTESIAN_POINT('Ctrl Pts',(13.8869929631353,-0.492919994478707,
4.32971322630275));
#13856=CARTESIAN_POINT('Ctrl Pts',(13.9106070792852,-0.590354424565592,
4.05623687359455));
#13857=CARTESIAN_POINT('Ctrl Pts',(13.934221195435,-0.546306307148498,3.76928296264551));
#13858=CARTESIAN_POINT('Ctrl Pts',(13.9578353115849,-0.371332080200278,
3.53762199579782));
#13859=CARTESIAN_POINT('Ctrl Pts',(13.9814494277348,-0.107365535263851,
3.41677313642685));
#13860=CARTESIAN_POINT('Ctrl Pts',(14.0050635438846,0.182331907606365,3.43569865495067));
#13861=CARTESIAN_POINT('Ctrl Pts',(14.0286776600345,0.428332239544634,3.58986291910809));
#13862=CARTESIAN_POINT('Ctrl Pts',(14.0522917761844,0.571679768510432,3.8423193898042));
#13863=CARTESIAN_POINT('Ctrl Pts',(14.0759058923342,0.578020261296468,4.1325651164018));
#13864=CARTESIAN_POINT('Ctrl Pts',(14.0995200084841,0.445834174668256,4.39104069002309));
#13865=CARTESIAN_POINT('Ctrl Pts',(14.123134124634,0.206800824478305,4.55580064011384));
#13866=CARTESIAN_POINT('Ctrl Pts',(14.1467482407838,-0.0817937829083601,
4.58735909768505));
#13867=CARTESIAN_POINT('Ctrl Pts',(14.1703623569337,-0.350785940826847,
4.4781528586907));
#13868=CARTESIAN_POINT('Ctrl Pts',(14.1939764730836,-0.535709806086595,
4.25435395852733));
#13869=CARTESIAN_POINT('Ctrl Pts',(14.2175905892334,-0.59224708706053,3.96959736155895));
#13870=CARTESIAN_POINT('Ctrl Pts',(14.2412047053833,-0.506848230788112,
3.69212696853602));
#13871=CARTESIAN_POINT('Ctrl Pts',(14.2648188215332,-0.29997966766535,3.48844049071174));
#13872=CARTESIAN_POINT('Ctrl Pts',(14.288432937683,-0.0212188889266537,
3.40735281042717));
#13873=CARTESIAN_POINT('Ctrl Pts',(14.3120470538329,0.262627144255178,3.46829715474127));
#13874=CARTESIAN_POINT('Ctrl Pts',(14.3356611699828,0.483532754079872,3.65666778728498));
#13875=CARTESIAN_POINT('Ctrl Pts',(14.3592752861326,0.588556373354274,3.9273203746575));
#13876=CARTESIAN_POINT('Ctrl Pts',(14.3828894022825,0.55252836061433,4.21539114019081));
#13877=CARTESIAN_POINT('Ctrl Pts',(14.4065035184324,0.384083079916361,4.45184191956682));
#13878=CARTESIAN_POINT('Ctrl Pts',(14.4301176345822,0.123589615384189,4.58000563749418));
#13879=CARTESIAN_POINT('Ctrl Pts',(14.4537317507321,-0.166522960823891,
4.56916696678068));
#13880=CARTESIAN_POINT('Ctrl Pts',(14.477345866882,-0.416727150247931,4.42192347031433));
#13881=CARTESIAN_POINT('Ctrl Pts',(14.5009599830318,-0.567059777136274,
4.17356307703535));
#13882=CARTESIAN_POINT('Ctrl Pts',(14.5245740991817,-0.58149258093928,3.88360708411314));
#13883=CARTESIAN_POINT('Ctrl Pts',(14.5481882153316,-0.456566639753037,
3.62154546373458));
#13884=CARTESIAN_POINT('Ctrl Pts',(14.5718023314814,-0.222221325036472,
3.45018310752014));
#13885=CARTESIAN_POINT('Ctrl Pts',(14.5954164476313,0.0653808771856868,
3.41058819705396));
#13886=CARTESIAN_POINT('Ctrl Pts',(14.6190305637812,0.337314097045906,3.51224992824993));
#13887=CARTESIAN_POINT('Ctrl Pts',(14.642644679931,0.528407645404381,3.73080435955289));
#13888=CARTESIAN_POINT('Ctrl Pts',(14.6662587960809,0.592864623089856,4.0138734000105));
#13889=CARTESIAN_POINT('Ctrl Pts',(14.6898729122308,0.515237466779568,4.29361758366474));
#13890=CARTESIAN_POINT('Ctrl Pts',(14.7134870283806,0.314130064687094,4.5029942692369));
#13891=CARTESIAN_POINT('Ctrl Pts',(14.7371011445305,0.0377392060970651,
4.59182487707066));
#13892=CARTESIAN_POINT('Ctrl Pts',(14.7607152606804,-0.24769611652869,4.53882053236973));
#13893=CARTESIAN_POINT('Ctrl Pts',(14.7843293768302,-0.47376933929102,4.35668409799883));
#13894=CARTESIAN_POINT('Ctrl Pts',(14.8079434929801,-0.586300444482135,
4.08906583263515));
#13895=CARTESIAN_POINT('Ctrl Pts',(14.83155760913,-0.558320561021625,3.80010232883727));
#13896=CARTESIAN_POINT('Ctrl Pts',(14.8551717252798,-0.396535280656446,
3.55904567554761));
#13897=CARTESIAN_POINT('Ctrl Pts',(14.8787858414297,-0.139717533720287,
3.42366683418339));
#13898=CARTESIAN_POINT('Ctrl Pts',(14.9023999575795,0.150584436790342,3.42641016570609));
#13899=CARTESIAN_POINT('Ctrl Pts',(14.9260140737294,0.404797918804129,3.56661847040663));
#13900=CARTESIAN_POINT('Ctrl Pts',(14.9496281898793,0.561998504794314,3.8106892976029));
#13901=CARTESIAN_POINT('Ctrl Pts',(14.9732423060292,0.584512788988964,4.10013056240029));
#13902=CARTESIAN_POINT('Ctrl Pts',(14.996856422179,0.466943341203511,4.36557310620026));
#13903=CARTESIAN_POINT('Ctrl Pts',(15.0204705383289,0.237470236409271,4.54340722946861));
#13904=CARTESIAN_POINT('Ctrl Pts',(15.0440846544788,-0.0489194860211801,
4.59100207336435));
#13905=CARTESIAN_POINT('Ctrl Pts',(15.0676987706286,-0.323572659684198,
4.49697628347096));
#13906=CARTESIAN_POINT('Ctrl Pts',(15.0913128867785,-0.520699184418956,
4.28381019498893));
#13907=CARTESIAN_POINT('Ctrl Pts',(15.1070556308784,-0.568863891700195,
4.09641102894772));
#13908=CARTESIAN_POINT('Ctrl Pts',(15.1149270029284,-0.569285911151507,
4.00255990244131));
#13909=CARTESIAN_POINT('Ctrl Pts',(12.455218991215,-0.25415908175074,3.42901124252432));
#13910=CARTESIAN_POINT('Ctrl Pts',(12.4630903632649,-0.16002722803387,3.38711117848463));
#13911=CARTESIAN_POINT('Ctrl Pts',(12.4788331073648,0.0492725194893315,
3.35081398558546));
#13912=CARTESIAN_POINT('Ctrl Pts',(12.5024472235147,0.351538860016532,3.45200243701797));
#13913=CARTESIAN_POINT('Ctrl Pts',(12.5260613396645,0.569511032758309,3.68451895614546));
#13914=CARTESIAN_POINT('Ctrl Pts',(12.5496754558144,0.651018771792273,3.99264764559437));
#13915=CARTESIAN_POINT('Ctrl Pts',(12.5732895719643,0.576495013506714,4.3025367374363));
#13916=CARTESIAN_POINT('Ctrl Pts',(12.5969036881141,0.363815091701307,4.53992168461618));
#13917=CARTESIAN_POINT('Ctrl Pts',(12.620517804264,0.0639420851661475,4.64791024952038));
#13918=CARTESIAN_POINT('Ctrl Pts',(12.6441319204139,-0.251254027515963,
4.60062280024232));
#13919=CARTESIAN_POINT('Ctrl Pts',(12.6677460365637,-0.506235857616531,
4.40939182910775));
#13920=CARTESIAN_POINT('Ctrl Pts',(12.6913601527136,-0.639894509617229,
4.12004729681268));
#13921=CARTESIAN_POINT('Ctrl Pts',(12.7149742688635,-0.620198095551099,
3.8019325752266));
#13922=CARTESIAN_POINT('Ctrl Pts',(12.7385883850133,-0.451866840211785,
3.53128609963859));
#13923=CARTESIAN_POINT('Ctrl Pts',(12.7622025011632,-0.17524257447904,3.37297016902465));
#13924=CARTESIAN_POINT('Ctrl Pts',(12.7858166173131,0.143379805101228,3.36492630429559));
#13925=CARTESIAN_POINT('Ctrl Pts',(12.809430733463,0.42764021116234,3.50908227080648));
#13926=CARTESIAN_POINT('Ctrl Pts',(12.8330448496128,0.609413666055986,3.77089008898231));
#13927=CARTESIAN_POINT('Ctrl Pts',(12.8566589657627,0.645136892431096,4.08760569204938));
#13928=CARTESIAN_POINT('Ctrl Pts',(12.8802730819125,0.526248572038732,4.38332598125533));
#13929=CARTESIAN_POINT('Ctrl Pts',(12.9038871980624,0.281241117720374,4.58717953054897));
#13930=CARTESIAN_POINT('Ctrl Pts',(12.9275013142123,-0.0311677281609838,
4.65031141781114));
#13931=CARTESIAN_POINT('Ctrl Pts',(12.9511154303622,-0.336107011072318,
4.55759164674784));
#13932=CARTESIAN_POINT('Ctrl Pts',(12.974729546512,-0.56049590900091,4.33124115596169));
#13933=CARTESIAN_POINT('Ctrl Pts',(12.9983436626619,-0.650558060547343,
4.02550641626558));
#13934=CARTESIAN_POINT('Ctrl Pts',(13.0219577788117,-0.584709444123524,
3.71365888635357));
#13935=CARTESIAN_POINT('Ctrl Pts',(13.0455718949616,-0.378731139057797,
3.47043499764384));
#13936=CARTESIAN_POINT('Ctrl Pts',(13.0691860111115,-0.0819872800401352,
3.35412504823007));
#13937=CARTESIAN_POINT('Ctrl Pts',(13.0928001272613,0.234405401379786,3.39260352716186));
#13938=CARTESIAN_POINT('Ctrl Pts',(13.1164142434112,0.494621196584012,3.57664879910166));
#13939=CARTESIAN_POINT('Ctrl Pts',(13.1400283595611,0.636297578801308,3.86215313342763));
#13940=CARTESIAN_POINT('Ctrl Pts',(13.1636424757109,0.625480816776257,4.18069342892634));
#13941=CARTESIAN_POINT('Ctrl Pts',(13.1872565918608,0.464763222827219,4.45592928631477));
#13942=CARTESIAN_POINT('Ctrl Pts',(13.2108707080107,0.192661887153653,4.62189851635989));
#13943=CARTESIAN_POINT('Ctrl Pts',(13.2344848241605,-0.125612210960856,
4.63882543771344));
#13944=CARTESIAN_POINT('Ctrl Pts',(13.2580989403104,-0.413782468289504,
4.50265339583901));
#13945=CARTESIAN_POINT('Ctrl Pts',(13.2817130564603,-0.602786876612853,
4.24601696851145));
#13946=CARTESIAN_POINT('Ctrl Pts',(13.3053271726101,-0.647329213752593,
3.9304208620728));
#13947=CARTESIAN_POINT('Ctrl Pts',(13.32894128876,-0.536734598538914,3.6314998804023));
#13948=CARTESIAN_POINT('Ctrl Pts',(13.3525554049099,-0.297507800394296,
3.42089251764738));
#13949=CARTESIAN_POINT('Ctrl Pts',(13.3761695210598,0.0130188131672444,
3.34907229440132));
#13950=CARTESIAN_POINT('Ctrl Pts',(13.3997836372096,0.320425377524893,3.43325142712992));
#13951=CARTESIAN_POINT('Ctrl Pts',(13.4233977533595,0.551039769569266,3.65325580067535));
#13952=CARTESIAN_POINT('Ctrl Pts',(13.4470118695093,0.649593644862141,3.95635983539258));
#13953=CARTESIAN_POINT('Ctrl Pts',(13.4706259856592,0.592467881122722,4.26992253935193));
#13954=CARTESIAN_POINT('Ctrl Pts',(13.4942401018091,0.393353065302923,4.5187964277335));
#13955=CARTESIAN_POINT('Ctrl Pts',(13.5178542179589,0.0999684491195412,
4.64333714069132));
#13956=CARTESIAN_POINT('Ctrl Pts',(13.5414683341088,-0.217374301809525,
4.61369762939502));
#13957=CARTESIAN_POINT('Ctrl Pts',(13.5650824502587,-0.482621788093898,
4.43698120905743));
#13958=CARTESIAN_POINT('Ctrl Pts',(13.5886965664085,-0.632205603168059,
4.15553919999523));
#13959=CARTESIAN_POINT('Ctrl Pts',(13.6123106825584,-0.630276944445953,
3.83682113889318));
#13960=CARTESIAN_POINT('Ctrl Pts',(13.6359247987083,-0.477298028416376,
3.55721002779864));
#13961=CARTESIAN_POINT('Ctrl Pts',(13.6595389148582,-0.209931317243796,
3.38371661595291));
#13962=CARTESIAN_POINT('Ctrl Pts',(13.683153031008,0.107746895509167,3.35791980725116));
#13963=CARTESIAN_POINT('Ctrl Pts',(13.7067671471579,0.399602814690774,3.48600198647908));
#13964=CARTESIAN_POINT('Ctrl Pts',(13.7303812633077,0.59569113756138,3.73726736776131));
#13965=CARTESIAN_POINT('Ctrl Pts',(13.7539953794576,0.649017932507905,4.05149845333026));
#13966=CARTESIAN_POINT('Ctrl Pts',(13.7776094956075,0.546803061895555,4.35338757606046));
#13967=CARTESIAN_POINT('Ctrl Pts',(13.8012236117573,0.313543031018869,4.57058490613733));
#13968=CARTESIAN_POINT('Ctrl Pts',(13.8248377279072,0.00514023007941788,
4.65103759142385));
#13969=CARTESIAN_POINT('Ctrl Pts',(13.8484518440571,-0.304494462781446,
4.57546458583277));
#13970=CARTESIAN_POINT('Ctrl Pts',(13.8720659602069,-0.541154937947787,
4.36197748624323));
#13971=CARTESIAN_POINT('Ctrl Pts',(13.8956800763568,-0.648123865072376,
4.06173996222779));
#13972=CARTESIAN_POINT('Ctrl Pts',(13.9192941925067,-0.599765396122921,
3.74670602647169));
#13973=CARTESIAN_POINT('Ctrl Pts',(13.9429083086565,-0.407668974822819,
3.49237575473668));
#13974=CARTESIAN_POINT('Ctrl Pts',(13.9665224248064,-0.117871845784803,
3.35970116712309));
#13975=CARTESIAN_POINT('Ctrl Pts',(13.9901365409563,0.200174091641329,3.38047865214521));
#13976=CARTESIAN_POINT('Ctrl Pts',(14.0137506571061,0.470246914526057,3.54972874087838));
#13977=CARTESIAN_POINT('Ctrl Pts',(14.037364773256,0.627621790796785,3.82688947135059));
#13978=CARTESIAN_POINT('Ctrl Pts',(14.0609788894059,0.634582735815489,4.14553734509456));
#13979=CARTESIAN_POINT('Ctrl Pts',(14.0845930055557,0.489461510650943,4.42930618095194));
#13980=CARTESIAN_POINT('Ctrl Pts',(14.1082071217056,0.227037427151766,4.61018880199865));
#13981=CARTESIAN_POINT('Ctrl Pts',(14.1318212378555,-0.0897977562486571,
4.64483542891575));
#13982=CARTESIAN_POINT('Ctrl Pts',(14.1554353540053,-0.385112282251534,
4.52494275637564));
#13983=CARTESIAN_POINT('Ctrl Pts',(14.1790494701552,-0.588131968915973,
4.27924389796604));
#13984=CARTESIAN_POINT('Ctrl Pts',(14.2026635863051,-0.65020173504413,3.96662229549764));
#13985=CARTESIAN_POINT('Ctrl Pts',(14.2262777024549,-0.556446129094758,
3.66199989226673));
#13986=CARTESIAN_POINT('Ctrl Pts',(14.2498918186048,-0.329334334698108,
3.43838156778717));
#13987=CARTESIAN_POINT('Ctrl Pts',(14.2735059347547,-0.0232952743833569,
3.34935901020328));
#13988=CARTESIAN_POINT('Ctrl Pts',(14.2971200509045,0.28832666060365,3.41626709515619));
#13989=CARTESIAN_POINT('Ctrl Pts',(14.3207341670544,0.530849104237583,3.62307083431711));
#13990=CARTESIAN_POINT('Ctrl Pts',(14.3443482832043,0.646149864620809,3.92020827196535));
#13991=CARTESIAN_POINT('Ctrl Pts',(14.3679623993541,0.606596311879891,4.2364683526943));
#13992=CARTESIAN_POINT('Ctrl Pts',(14.391576515504,0.42166773027486,4.49605714656388));
#13993=CARTESIAN_POINT('Ctrl Pts',(14.4151906316539,0.135683541737747,4.63676239203782));
#13994=CARTESIAN_POINT('Ctrl Pts',(14.4388047478037,-0.182818152115814,
4.62486309754155));
#13995=CARTESIAN_POINT('Ctrl Pts',(14.4624188639536,-0.457506203155893,
4.46321101183598));
#13996=CARTESIAN_POINT('Ctrl Pts',(14.4860329801035,-0.622549707754089,
4.19054718257559));
#13997=CARTESIAN_POINT('Ctrl Pts',(14.5096470962533,-0.63839484111024,3.87221739454711));
#13998=CARTESIAN_POINT('Ctrl Pts',(14.5332612124032,-0.501244206711231,
3.58451159745434));
#13999=CARTESIAN_POINT('Ctrl Pts',(14.5568753285531,-0.243966908844842,
3.39638048838484));
#14000=CARTESIAN_POINT('Ctrl Pts',(14.5804894447029,0.0717787570654544,
3.35291099727801));
#14001=CARTESIAN_POINT('Ctrl Pts',(14.6041035608528,0.370322144162233,3.46452089026927));
#14002=CARTESIAN_POINT('Ctrl Pts',(14.6277176770027,0.580115251486915,3.70446207957941));
#14003=CARTESIAN_POINT('Ctrl Pts',(14.6513317931525,0.650879700384091,4.0152309888134));
#14004=CARTESIAN_POINT('Ctrl Pts',(14.6749459093024,0.565656298155129,4.32234968564526));
#14005=CARTESIAN_POINT('Ctrl Pts',(14.6985600254523,0.344869426209941,4.55221503612336));
#14006=CARTESIAN_POINT('Ctrl Pts',(14.7221741416021,0.041432195817608,4.64973820947522));
#14007=CARTESIAN_POINT('Ctrl Pts',(14.745788257752,-0.271934549361806,4.59154709694401));
#14008=CARTESIAN_POINT('Ctrl Pts',(14.7694023739019,-0.520130285395982,
4.39158760667368));
#14009=CARTESIAN_POINT('Ctrl Pts',(14.7930164900517,-0.64367318065081,4.09778141619902));
#14010=CARTESIAN_POINT('Ctrl Pts',(14.8166306062016,-0.612955311082805,
3.78054123783642));
#14011=CARTESIAN_POINT('Ctrl Pts',(14.8402447223515,-0.435338447621071,
3.51589585985611));
#14012=CARTESIAN_POINT('Ctrl Pts',(14.8638588385013,-0.153389665944836,
3.36726945127358));
#14013=CARTESIAN_POINT('Ctrl Pts',(14.8874729546512,0.165319955489652,3.37028123293502));
#14014=CARTESIAN_POINT('Ctrl Pts',(14.9110870708011,0.444409630539555,3.52420969451069));
#14015=CARTESIAN_POINT('Ctrl Pts',(14.9347011869509,0.616993161964042,3.79216419995926));
#14016=CARTESIAN_POINT('Ctrl Pts',(14.9583153031008,0.641710593195818,4.10992889087348));
#14017=CARTESIAN_POINT('Ctrl Pts',(14.9819294192507,0.512636325700993,4.40134645341462));
#14018=CARTESIAN_POINT('Ctrl Pts',(15.0055435354005,0.260708010403211,4.59658262768273));
#14019=CARTESIAN_POINT('Ctrl Pts',(15.0291576515504,-0.0537065278721878,
4.64883488988255));
#14020=CARTESIAN_POINT('Ctrl Pts',(15.0527717677003,-0.355236031271534,
4.54560815721762));
#14021=CARTESIAN_POINT('Ctrl Pts',(15.0763858838501,-0.571652475026301,
4.31158258982903));
#14022=CARTESIAN_POINT('Ctrl Pts',(15.09212862795,-0.624530364890795,4.10584538053252));
#14023=CARTESIAN_POINT('Ctrl Pts',(15.1,-0.624993681275899,4.00281040303152));
#14024=CARTESIAN_POINT('Ctrl Pts',(15.1,-0.624993681275899,4.00281040303152));
#14025=CARTESIAN_POINT('Ctrl Pts',(15.1,-0.617358358083874,4.02914127082806));
#14026=CARTESIAN_POINT('Ctrl Pts',(15.1,-0.607931963506944,4.05484759228836));
#14027=CARTESIAN_POINT('Ctrl Pts',(15.1,-0.596773861259576,4.07974656001827));
#14028=CARTESIAN_POINT('Ctrl Pts',(15.1,-0.585871522029423,4.10407480030985));
#14029=CARTESIAN_POINT('Ctrl Pts',(15.1,-0.573314772633929,4.12763281365198));
#14030=CARTESIAN_POINT('Ctrl Pts',(15.1,-0.559143639302279,4.1502040881484));
#14031=CARTESIAN_POINT('Ctrl Pts',(15.1,-0.549626121151564,4.16536325076984));
#14032=CARTESIAN_POINT('Ctrl Pts',(15.1,-0.539380106047495,4.18007635520315));
#14033=CARTESIAN_POINT('Ctrl Pts',(15.1,-0.528417753985571,4.19426420824267));
#14034=CARTESIAN_POINT('Ctrl Pts',(15.1,-0.523814643226911,4.2002217124899));
#14035=CARTESIAN_POINT('Ctrl Pts',(15.1,-0.519084627089791,4.20608691507751));
#14036=CARTESIAN_POINT('Ctrl Pts',(15.1,-0.514239086396905,4.21184190560023));
#14037=CARTESIAN_POINT('Ctrl Pts',(15.1,-0.50085552272952,4.2277374035328));
#14038=CARTESIAN_POINT('Ctrl Pts',(15.1,-0.486572803760524,4.24281789068328));
#14039=CARTESIAN_POINT('Ctrl Pts',(15.1,-0.4714177983537,4.25697008589974));
#14040=CARTESIAN_POINT('Ctrl Pts',(15.1,-0.457151696655403,4.27029219637033));
#14041=CARTESIAN_POINT('Ctrl Pts',(15.1,-0.442112042545397,4.28279146400573));
#14042=CARTESIAN_POINT('Ctrl Pts',(15.1,-0.426369607892924,4.29437520287289));
#14043=CARTESIAN_POINT('Ctrl Pts',(15.1,-0.419074661497203,4.29974303548351));
#14044=CARTESIAN_POINT('Ctrl Pts',(15.1,-0.411628924918527,4.30491398987477));
#14045=CARTESIAN_POINT('Ctrl Pts',(15.1,-0.404040271526401,4.30987739070861));
#14046=CARTESIAN_POINT('Ctrl Pts',(15.1,-0.398073367501634,4.31378007737535));
#14047=CARTESIAN_POINT('Ctrl Pts',(15.1,-0.392026704362881,4.31754881952869));
#14048=CARTESIAN_POINT('Ctrl Pts',(15.1,-0.385904261325812,4.32117966642505));
#14049=CARTESIAN_POINT('Ctrl Pts',(15.1,-0.366868686798561,4.33246850264191));
#14050=CARTESIAN_POINT('Ctrl Pts',(15.1,-0.347097727375919,4.34242824684389));
#14051=CARTESIAN_POINT('Ctrl Pts',(15.1,-0.326713262272485,4.3509180109496));
#14052=CARTESIAN_POINT('Ctrl Pts',(15.1,-0.308010762698638,4.35870726657947));
#14053=CARTESIAN_POINT('Ctrl Pts',(15.1,-0.288791261952878,4.36525839133365));
#14054=CARTESIAN_POINT('Ctrl Pts',(15.1,-0.269173508333929,4.37043259773196));
#14055=CARTESIAN_POINT('Ctrl Pts',(12.5,-0.186196943290592,3.58169363627332));
#14056=CARTESIAN_POINT('Ctrl Pts',(12.5,-0.170588484282379,3.56594316788148));
#14057=CARTESIAN_POINT('Ctrl Pts',(12.5,-0.153797667832464,3.55144458439849));
#14058=CARTESIAN_POINT('Ctrl Pts',(12.5,-0.136060690067392,3.53823162417247));
#14059=CARTESIAN_POINT('Ctrl Pts',(12.5,-0.117990710310259,3.5247705978929));
#14060=CARTESIAN_POINT('Ctrl Pts',(12.5,-0.0989385549429972,3.51264262455394));
#14061=CARTESIAN_POINT('Ctrl Pts',(12.5,-0.0790990435859813,3.5018744512649));
#14062=CARTESIAN_POINT('Ctrl Pts',(12.5,-0.0668145727052721,3.49520688224936));
#14063=CARTESIAN_POINT('Ctrl Pts',(12.5,-0.054227138249592,3.4890605701039));
#14064=CARTESIAN_POINT('Ctrl Pts',(12.5,-0.0413735013057162,3.4834433907237));
#14065=CARTESIAN_POINT('Ctrl Pts',(12.5,-0.0353493612034326,3.48081077586818));
#14066=CARTESIAN_POINT('Ctrl Pts',(12.5,-0.0292710672153644,3.47829647656688));
#14067=CARTESIAN_POINT('Ctrl Pts',(12.5,-0.0231507758853709,3.47590397706369));
#14068=CARTESIAN_POINT('Ctrl Pts',(12.5,-0.00211397253512804,3.467680423829));
#14069=CARTESIAN_POINT('Ctrl Pts',(12.5,0.0194422610390746,3.46088402724794));
#14070=CARTESIAN_POINT('Ctrl Pts',(12.5,0.0413436963816045,3.45552737346533));
#14071=CARTESIAN_POINT('Ctrl Pts',(12.5,0.0650920698750741,3.44971899548849));
#14072=CARTESIAN_POINT('Ctrl Pts',(12.5,0.089246474293393,3.44560199012534));
#14073=CARTESIAN_POINT('Ctrl Pts',(12.5,0.113633446029948,3.44311473184586));
#14074=CARTESIAN_POINT('Ctrl Pts',(12.5,0.123118497624279,3.44214733936417));
#14075=CARTESIAN_POINT('Ctrl Pts',(12.5,0.132642564327611,3.44142688205345));
#14076=CARTESIAN_POINT('Ctrl Pts',(12.5,0.142169452875131,3.44095138714122));
#14077=CARTESIAN_POINT('Ctrl Pts',(12.5,0.170359862108328,3.43954438042575));
#14078=CARTESIAN_POINT('Ctrl Pts',(12.5,0.19861482332424,3.44027367679077));
#14079=CARTESIAN_POINT('Ctrl Pts',(12.5,0.226679319731597,3.44302987267532));
#14080=CARTESIAN_POINT('Ctrl Pts',(12.5,0.254743816138955,3.44578606855986));
#14081=CARTESIAN_POINT('Ctrl Pts',(12.5,0.282619254593541,3.45056842907764));
#14082=CARTESIAN_POINT('Ctrl Pts',(12.5,0.310093463203745,3.45730861053194));
#14083=CARTESIAN_POINT('Ctrl Pts',(15.0699957084852,-1.05870731373636E-5,
4.45788944868556));
#14084=CARTESIAN_POINT('Ctrl Pts',(15.0634386537186,0.0628625045491076,
4.45782850550181));
#14085=CARTESIAN_POINT('Ctrl Pts',(15.0568815989521,0.125761012144406,4.44477074790967));
#14086=CARTESIAN_POINT('Ctrl Pts',(15.0503245441856,0.183365120595825,4.41959809737683));
#14087=CARTESIAN_POINT('Ctrl Pts',(15.0424531721356,0.252515583017112,4.38937975928409));
#14088=CARTESIAN_POINT('Ctrl Pts',(15.0345818000857,0.314036477612831,4.34170308552782));
#14089=CARTESIAN_POINT('Ctrl Pts',(15.0267104280357,0.360556892971808,4.28228266426341));
#14090=CARTESIAN_POINT('Ctrl Pts',(15.0188390559858,0.407077308330786,4.222862242999));
#14091=CARTESIAN_POINT('Ctrl Pts',(15.0109676839358,0.438597244453022,4.15169807422645));
#14092=CARTESIAN_POINT('Ctrl Pts',(15.0030963118859,0.45133921416074,4.07731692107955));
#14093=CARTESIAN_POINT('Ctrl Pts',(14.9952249398359,0.464081183868457,4.00293576793266));
#14094=CARTESIAN_POINT('Ctrl Pts',(14.9873535677859,0.458045187161657,3.92533763041141));
#14095=CARTESIAN_POINT('Ctrl Pts',(14.979482195736,0.433954739621328,3.85382131653551));
#14096=CARTESIAN_POINT('Ctrl Pts',(14.971610823686,0.409864292080999,3.78230500265962));
#14097=CARTESIAN_POINT('Ctrl Pts',(14.9637394516361,0.367719393707138,3.71687051242907));
#14098=CARTESIAN_POINT('Ctrl Pts',(14.9558680795861,0.312570095196614,3.66535860215541));
#14099=CARTESIAN_POINT('Ctrl Pts',(14.9479967075362,0.257420796686091,3.61384669188175));
#14100=CARTESIAN_POINT('Ctrl Pts',(14.9401253354862,0.189267098038905,3.57625736156498));
#14101=CARTESIAN_POINT('Ctrl Pts',(14.9322539634362,0.116275803938161,3.55709495786573));
#14102=CARTESIAN_POINT('Ctrl Pts',(14.9243825913863,0.0432845098374172,
3.53793255416647));
#14103=CARTESIAN_POINT('Ctrl Pts',(14.9165112193363,-0.0345443797168851,
3.53719707708475));
#14104=CARTESIAN_POINT('Ctrl Pts',(14.9086398472864,-0.107884770736704,
3.55497662303181));
#14105=CARTESIAN_POINT('Ctrl Pts',(14.9007684752364,-0.181225161756525,
3.57275616897888));
#14106=CARTESIAN_POINT('Ctrl Pts',(14.8928971031865,-0.250077054241862,
3.60905073795473));
#14107=CARTESIAN_POINT('Ctrl Pts',(14.8850257311365,-0.306190019513209,
3.65951122309406));
#14108=CARTESIAN_POINT('Ctrl Pts',(14.8771543590866,-0.362302984784554,
3.70997170823338));
#14109=CARTESIAN_POINT('Ctrl Pts',(14.8692829870366,-0.405677022841909,
3.77459810953617));
#14110=CARTESIAN_POINT('Ctrl Pts',(14.8614116149867,-0.431114693744839,
3.84564633596564));
#14111=CARTESIAN_POINT('Ctrl Pts',(14.8535402429367,-0.45655236464777,3.91669456239511));
#14112=CARTESIAN_POINT('Ctrl Pts',(14.8456688708867,-0.464053668396277,
3.99416461395126));
#14113=CARTESIAN_POINT('Ctrl Pts',(14.8377974988368,-0.452719732759917,
4.06877337558629));
#14114=CARTESIAN_POINT('Ctrl Pts',(14.8299261267868,-0.441385797123556,
4.14338213722132));
#14115=CARTESIAN_POINT('Ctrl Pts',(14.8220547547369,-0.411216622102327,
4.21512960893523));
#14116=CARTESIAN_POINT('Ctrl Pts',(14.8141833826869,-0.365827335221939,
4.27541839855419));
#14117=CARTESIAN_POINT('Ctrl Pts',(14.806312010637,-0.32043804834155,4.33570718817315));
#14118=CARTESIAN_POINT('Ctrl Pts',(14.798440638587,-0.259828649602004,4.38453729569717));
#14119=CARTESIAN_POINT('Ctrl Pts',(14.7905692665371,-0.191261870645823,
4.41605748429924));
#14120=CARTESIAN_POINT('Ctrl Pts',(14.7837114138531,-0.131523763221734,
4.44351912740692));
#14121=CARTESIAN_POINT('Ctrl Pts',(14.7768535611691,-0.065745536276614,
4.45784152413683));
#14122=CARTESIAN_POINT('Ctrl Pts',(14.7699957084852,8.6346448269735E-6,
4.45789857801605));
#14123=CARTESIAN_POINT('Ctrl Pts',(12.5,0.310062960217722,4.54266560670548));
#14124=CARTESIAN_POINT('Ctrl Pts',(12.50787137205,0.220600394030941,4.59378185169648));
#14125=CARTESIAN_POINT('Ctrl Pts',(12.5236141161499,0.0159878432799406,
4.65085692712531));
#14126=CARTESIAN_POINT('Ctrl Pts',(12.5472282322997,-0.294892507759568,
4.580447501361));
#14127=CARTESIAN_POINT('Ctrl Pts',(12.5708423484496,-0.535054221536356,
4.37092866956447));
#14128=CARTESIAN_POINT('Ctrl Pts',(12.5944564645995,-0.647009713430093,
4.07251155115386));
#14129=CARTESIAN_POINT('Ctrl Pts',(12.6180705807493,-0.603894380709874,
3.75671714932517));
#14130=CARTESIAN_POINT('Ctrl Pts',(12.6416846968992,-0.416056506175611,
3.49922677321964));
#14131=CARTESIAN_POINT('Ctrl Pts',(12.6652988130491,-0.128505496873939,
3.36175035317655));
#14132=CARTESIAN_POINT('Ctrl Pts',(12.6889129291989,0.189841674427298,3.37723482234205));
#14133=CARTESIAN_POINT('Ctrl Pts',(12.7125270453488,0.462692468193658,3.54196933898577));
#14134=CARTESIAN_POINT('Ctrl Pts',(12.7361411614987,0.624655556881011,3.81647407445394));
#14135=CARTESIAN_POINT('Ctrl Pts',(12.7597552776485,0.636915702199809,4.13496208375113));
#14136=CARTESIAN_POINT('Ctrl Pts',(12.7833693937984,0.496534514683115,4.42110548633398));
#14137=CARTESIAN_POINT('Ctrl Pts',(12.8069835099483,0.237155397994168,4.60632802944461));
#14138=CARTESIAN_POINT('Ctrl Pts',(12.8305976260981,-0.0790596718614395,
4.64623983861064));
#14139=CARTESIAN_POINT('Ctrl Pts',(12.854211742248,-0.376327535803878,4.5312757721487));
#14140=CARTESIAN_POINT('Ctrl Pts',(12.8778258583979,-0.583405888470749,
4.28898776831928));
#14141=CARTESIAN_POINT('Ctrl Pts',(12.9014399745477,-0.650666957548692,
3.97744183415536));
#14142=CARTESIAN_POINT('Ctrl Pts',(12.9250540906976,-0.561991161265395,
3.67130212143154));
#14143=CARTESIAN_POINT('Ctrl Pts',(12.9486682068475,-0.338630270727757,
3.44393714350224));
#14144=CARTESIAN_POINT('Ctrl Pts',(12.9722823229973,-0.0341142786054444,
3.34983650006563));
#14145=CARTESIAN_POINT('Ctrl Pts',(12.9958964391472,0.278577437919422,3.41155206540036));
#14146=CARTESIAN_POINT('Ctrl Pts',(13.0195105552971,0.524506132150044,3.61429327464512));
#14147=CARTESIAN_POINT('Ctrl Pts',(13.0431246714469,0.644733280558021,3.90947178565704));
#14148=CARTESIAN_POINT('Ctrl Pts',(13.0667387875968,0.61044561006836,4.22634601343335));
#14149=CARTESIAN_POINT('Ctrl Pts',(13.0903529037467,0.429860399609997,4.4889748434194));
#14150=CARTESIAN_POINT('Ctrl Pts',(13.1139670198965,0.146256151980267,4.63441744826062));
#14151=CARTESIAN_POINT('Ctrl Pts',(13.1375811360464,-0.172399400609521,
4.62781749523177));
#14152=CARTESIAN_POINT('Ctrl Pts',(13.1611952521963,-0.449738236712957,
4.47075670902068));
#14153=CARTESIAN_POINT('Ctrl Pts',(13.1848093683461,-0.619294173608025,
4.2008758003961));
#14154=CARTESIAN_POINT('Ctrl Pts',(13.208423484496,-0.64043195068177,3.88285360784221));
#14155=CARTESIAN_POINT('Ctrl Pts',(13.2320376006459,-0.508085752511173,
3.59290636366459));
#14156=CARTESIAN_POINT('Ctrl Pts',(13.2556517167957,-0.253973266794505,
3.40052194335125));
#14157=CARTESIAN_POINT('Ctrl Pts',(13.2792658329456,0.0610056803032868,
3.3518066124833));
#14158=CARTESIAN_POINT('Ctrl Pts',(13.3028799490955,0.361364191435218,3.45843533922715));
#14159=CARTESIAN_POINT('Ctrl Pts',(13.3264940652453,0.575119258511334,3.69485380694));
#14160=CARTESIAN_POINT('Ctrl Pts',(13.3501081813952,0.65104299168552,4.00440268404554));
#14161=CARTESIAN_POINT('Ctrl Pts',(13.3737222975451,0.570939739771795,4.31289642727099));
#14162=CARTESIAN_POINT('Ctrl Pts',(13.3973364136949,0.354006804717113,4.54640236352309));
#14163=CARTESIAN_POINT('Ctrl Pts',(13.4209505298448,0.0522336745508671,
4.6489591696652));
#14164=CARTESIAN_POINT('Ctrl Pts',(13.4445646459947,-0.26205761933777,4.59598839317277));
#14165=CARTESIAN_POINT('Ctrl Pts',(13.4681787621445,-0.513544980480383,
4.40018484937968));
#14166=CARTESIAN_POINT('Ctrl Pts',(13.4917928782944,-0.64195771209056,4.10847422061066));
#14167=CARTESIAN_POINT('Ctrl Pts',(13.5154069944443,-0.616520809113462,
3.79076698974655));
#14168=CARTESIAN_POINT('Ctrl Pts',(13.5390211105941,-0.443330402422436,
3.52320390633144));
#14169=CARTESIAN_POINT('Ctrl Pts',(13.562635226744,-0.163892778617988,3.36990832590288));
#14170=CARTESIAN_POINT('Ctrl Pts',(13.5862493428939,0.154822890495328,3.36761860145296));
#14171=CARTESIAN_POINT('Ctrl Pts',(13.6098634590437,0.43643417612693,3.51688348138565));
#14172=CARTESIAN_POINT('Ctrl Pts',(13.6334775751936,0.613450973283793,3.78193059814177));
#14173=CARTESIAN_POINT('Ctrl Pts',(13.6570916913435,0.643449974253473,4.09923956510808));
#14174=CARTESIAN_POINT('Ctrl Pts',(13.6807058074933,0.519241709620395,4.39276507945606));
#14175=CARTESIAN_POINT('Ctrl Pts',(13.7043199236432,0.270593554659618,4.59216170834183));
#14176=CARTESIAN_POINT('Ctrl Pts',(13.7279340397931,-0.0429042293685969,
4.64964266158552));
#14177=CARTESIAN_POINT('Ctrl Pts',(13.7515481559429,-0.346119716157775,
4.55143222859795));
#14178=CARTESIAN_POINT('Ctrl Pts',(13.7751622720928,-0.566385203513325,
4.32106722332061));
#14179=CARTESIAN_POINT('Ctrl Pts',(13.7987763882427,-0.650912534047929,
4.01375622291695));
#14180=CARTESIAN_POINT('Ctrl Pts',(13.8223905043925,-0.57944414457563,3.70314844792952));
#14181=CARTESIAN_POINT('Ctrl Pts',(13.8460046205424,-0.369107932149097,
3.46368321387984));
#14182=CARTESIAN_POINT('Ctrl Pts',(13.8696187366923,-0.0703124342978696,
3.35275003110641));
#14183=CARTESIAN_POINT('Ctrl Pts',(13.8932328528421,0.245333927901481,3.3969348091043));
#14184=CARTESIAN_POINT('Ctrl Pts',(13.916846968992,0.502184306426786,3.58564835824111));
#14185=CARTESIAN_POINT('Ctrl Pts',(13.9404610851419,0.638682720042094,3.87366416276737));
#14186=CARTESIAN_POINT('Ctrl Pts',(13.9640752012917,0.62211637371287,4.19195723015293));
#14187=CARTESIAN_POINT('Ctrl Pts',(13.9876893174416,0.456455507660852,4.46424641105313));
#14188=CARTESIAN_POINT('Ctrl Pts',(14.0113034335915,0.181401901656729,4.62527570776815));
#14189=CARTESIAN_POINT('Ctrl Pts',(14.0349175497413,-0.137125932879425,
4.63645332836083));
#14190=CARTESIAN_POINT('Ctrl Pts',(14.0585316658912,-0.422790583021024,
4.49510047824495));
#14191=CARTESIAN_POINT('Ctrl Pts',(14.0821457820411,-0.60713052675338,4.23509335195577));
#14192=CARTESIAN_POINT('Ctrl Pts',(14.1057598981909,-0.645967413308333,
3.91874446730605));
#14193=CARTESIAN_POINT('Ctrl Pts',(14.1293740143408,-0.529993712466286,
3.62186903671368));
#14194=CARTESIAN_POINT('Ctrl Pts',(14.1529881304907,-0.287003328966194,
3.41561532377041));
#14195=CARTESIAN_POINT('Ctrl Pts',(14.1766022466405,0.0247694002478971,
3.34941346658496));
#14196=CARTESIAN_POINT('Ctrl Pts',(14.2002163627904,0.330605970264406,3.43912920108534));
#14197=CARTESIAN_POINT('Ctrl Pts',(14.2238304789403,0.557210518047066,3.66326152695696));
#14198=CARTESIAN_POINT('Ctrl Pts',(14.2474445950901,0.650275686248857,3.96809557204375));
#14199=CARTESIAN_POINT('Ctrl Pts',(14.27105871124,0.587497759452106,4.28057573538778));
#14200=CARTESIAN_POINT('Ctrl Pts',(14.2946728273899,0.383921904832036,4.52581397056352));
#14201=CARTESIAN_POINT('Ctrl Pts',(14.3182869435397,0.088336493108731,4.64503722732482));
#14202=CARTESIAN_POINT('Ctrl Pts',(14.3419010596896,-0.22841937412829,4.6096728222354));
#14203=CARTESIAN_POINT('Ctrl Pts',(14.3655151758395,-0.490432948250941,
4.42819608115853));
#14204=CARTESIAN_POINT('Ctrl Pts',(14.3891292919893,-0.634910852255616,
4.14409916841427));
#14205=CARTESIAN_POINT('Ctrl Pts',(14.4127434081392,-0.627227950688033,
3.82546788683648));
#14206=CARTESIAN_POINT('Ctrl Pts',(14.4363575242891,-0.469225504392149,
3.54866444115539));
#14207=CARTESIAN_POINT('Ctrl Pts',(14.4599716404389,-0.198769899531221,
3.38002670405092));
#14208=CARTESIAN_POINT('Ctrl Pts',(14.4835857565888,0.11932229545683,3.35996988316441));
#14209=CARTESIAN_POINT('Ctrl Pts',(14.5071998727387,0.408818071695872,3.49330073524378));
#14210=CARTESIAN_POINT('Ctrl Pts',(14.5308139888885,0.600337751131954,3.74806559342675));
#14211=CARTESIAN_POINT('Ctrl Pts',(14.5544281050384,0.647982309355475,4.06320828594604));
#14212=CARTESIAN_POINT('Ctrl Pts',(14.5780422211883,0.540333396317157,4.36320267272319));
#14213=CARTESIAN_POINT('Ctrl Pts',(14.6016563373381,0.303189823409542,4.57615301060753));
#14214=CARTESIAN_POINT('Ctrl Pts',(14.625270453488,-0.00661530128860875,
4.65102426869959));
#14215=CARTESIAN_POINT('Ctrl Pts',(14.6488845696379,-0.314835022974042,
4.56987302880665));
#14216=CARTESIAN_POINT('Ctrl Pts',(14.6724986857877,-0.547602339746838,
4.35214775046202));
#14217=CARTESIAN_POINT('Ctrl Pts',(14.6961128019376,-0.649132943719538,
4.05002781234082));
#14218=CARTESIAN_POINT('Ctrl Pts',(14.7197269180875,-0.595094318970103,
3.73591836064326));
#14219=CARTESIAN_POINT('Ctrl Pts',(14.7433410342373,-0.398437197867616,
3.48509791236843));
#14220=CARTESIAN_POINT('Ctrl Pts',(14.7669551503872,-0.1062918289807,3.35767733339665));
#14221=CARTESIAN_POINT('Ctrl Pts',(14.7905692665371,0.211327117384507,3.38419385377023));
#14222=CARTESIAN_POINT('Ctrl Pts',(14.8141833826869,0.478300047385911,3.5582926020622));
#14223=CARTESIAN_POINT('Ctrl Pts',(14.8377974988368,0.630645044771057,3.83824960712979));
#14224=CARTESIAN_POINT('Ctrl Pts',(14.8614116149867,0.631851559871185,4.15697121131127));
#14225=CARTESIAN_POINT('Ctrl Pts',(14.8850257311365,0.481630465478622,4.4380735902585));
#14226=CARTESIAN_POINT('Ctrl Pts',(14.9086398472864,0.215983244330552,4.61418854455152));
#14227=CARTESIAN_POINT('Ctrl Pts',(14.9322539634363,-0.101425794369151,
4.64310902247508));
#14228=CARTESIAN_POINT('Ctrl Pts',(14.9558680795861,-0.394527586443172,
4.517903766532));
#14229=CARTESIAN_POINT('Ctrl Pts',(14.979482195736,-0.593077772790822,4.26857965265179));
#14230=CARTESIAN_POINT('Ctrl Pts',(15.0030963118859,-0.649493436571599,
3.95488773069898));
#14231=CARTESIAN_POINT('Ctrl Pts',(15.0267104280357,-0.550252000240565,
3.65200904506483));
#14232=CARTESIAN_POINT('Ctrl Pts',(15.0503245441856,-0.319142060764588,
3.43252503194012));
#14233=CARTESIAN_POINT('Ctrl Pts',(15.0739386603355,-0.0115409051696555,
3.34904846156061));
#14234=CARTESIAN_POINT('Ctrl Pts',(15.0975527764853,0.298810377697559,3.42155963907315));
#14235=CARTESIAN_POINT('Ctrl Pts',(15.1211668926352,0.537575400322941,3.63273573589665));
#14236=CARTESIAN_POINT('Ctrl Pts',(15.1369096367351,0.610790903144771,3.83214323401692));
#14237=CARTESIAN_POINT('Ctrl Pts',(15.1447810087851,0.621570310124627,3.93461384266089));
#14238=CARTESIAN_POINT('Ctrl Pts',(12.4850729970716,0.282426015030316,4.49429601229446));
#14239=CARTESIAN_POINT('Ctrl Pts',(12.4929443691216,0.200937545576316,4.54085609598193));
#14240=CARTESIAN_POINT('Ctrl Pts',(12.5086871132215,0.0145627935155885,
4.59284387968754));
#14241=CARTESIAN_POINT('Ctrl Pts',(12.5323012293714,-0.268607755567932,
4.52871028073968));
#14242=CARTESIAN_POINT('Ctrl Pts',(12.5559153455213,-0.487363055256749,
4.3378665608173));
#14243=CARTESIAN_POINT('Ctrl Pts',(12.5795294616711,-0.589339580973024,
4.06604835489435));
#14244=CARTESIAN_POINT('Ctrl Pts',(12.603143577821,-0.550067261575934,3.77840176074865));
#14245=CARTESIAN_POINT('Ctrl Pts',(12.6267576939709,-0.378972002925158,
3.54386236016666));
#14246=CARTESIAN_POINT('Ctrl Pts',(12.6503718101207,-0.117051373585908,
3.41863967169675));
#14247=CARTESIAN_POINT('Ctrl Pts',(12.6739859262706,0.172920453180012,3.43274395851062));
#14248=CARTESIAN_POINT('Ctrl Pts',(12.6976000424204,0.42145114619533,3.58279513857084));
#14249=CARTESIAN_POINT('Ctrl Pts',(12.7212141585703,0.568977924911017,3.83283235195095));
#14250=CARTESIAN_POINT('Ctrl Pts',(12.7448282747202,0.580145282610399,4.12293246335278));
#14251=CARTESIAN_POINT('Ctrl Pts',(12.76844239087,0.45227673827436,4.38357095065208));
#14252=CARTESIAN_POINT('Ctrl Pts',(12.7920565070199,0.216016946852954,4.55228399108678));
#14253=CARTESIAN_POINT('Ctrl Pts',(12.8156706231698,-0.0720128197761896,
4.58863832766248));
#14254=CARTESIAN_POINT('Ctrl Pts',(12.8392847393196,-0.34278420811256,4.48392139165784));
#14255=CARTESIAN_POINT('Ctrl Pts',(12.8628988554695,-0.531404976945056,
4.26322932523642));
#14256=CARTESIAN_POINT('Ctrl Pts',(12.8865129716194,-0.592670842732518,
3.97945251867098));
#14257=CARTESIAN_POINT('Ctrl Pts',(12.9101270877692,-0.51189901575794,3.70060005900794));
#14258=CARTESIAN_POINT('Ctrl Pts',(12.9337412039191,-0.308447025930223,
3.49350087944474));
#14259=CARTESIAN_POINT('Ctrl Pts',(12.957355320069,-0.0310735592390789,
3.40778774002645));
#14260=CARTESIAN_POINT('Ctrl Pts',(12.9809694362188,0.253746902286204,3.46400239130434));
#14261=CARTESIAN_POINT('Ctrl Pts',(13.0045835523687,0.477755152237737,3.64867260076509));
#14262=CARTESIAN_POINT('Ctrl Pts',(13.0281976685186,0.587266054150949,3.91754086716214));
#14263=CARTESIAN_POINT('Ctrl Pts',(13.0518117846685,0.556034558024266,4.20617103876933));
#14264=CARTESIAN_POINT('Ctrl Pts',(13.0754259008183,0.391545509324759,4.44539088570928));
#14265=CARTESIAN_POINT('Ctrl Pts',(13.0990400169682,0.133219853633759,4.57786970637232));
#14266=CARTESIAN_POINT('Ctrl Pts',(13.122654133118,-0.157032867368526,4.57185802915678));
#14267=CARTESIAN_POINT('Ctrl Pts',(13.1462682492679,-0.409651568547275,
4.42879659435664));
#14268=CARTESIAN_POINT('Ctrl Pts',(13.1698823654178,-0.564094419600429,
4.1829710707208));
#14269=CARTESIAN_POINT('Ctrl Pts',(13.1934964815676,-0.583348116144335,
3.89329525626321));
#14270=CARTESIAN_POINT('Ctrl Pts',(13.2171105977175,-0.462798375770677,
3.62919197644995));
#14271=CARTESIAN_POINT('Ctrl Pts',(13.2407247138674,-0.231335782947555,
3.45395542080054));
#14272=CARTESIAN_POINT('Ctrl Pts',(13.2643388300172,0.055568040665587,3.40958224975729));
#14273=CARTESIAN_POINT('Ctrl Pts',(13.2879529461671,0.329154596505292,3.50670680265737));
#14274=CARTESIAN_POINT('Ctrl Pts',(13.311567062317,0.523856961936024,3.72205250428141));
#14275=CARTESIAN_POINT('Ctrl Pts',(13.3351811784668,0.593013359693284,4.00401025814095));
#14276=CARTESIAN_POINT('Ctrl Pts',(13.3587952946167,0.520049977633468,4.28500692572024));
#14277=CARTESIAN_POINT('Ctrl Pts',(13.3824094107666,0.322452998189994,4.49769969952106));
#14278=CARTESIAN_POINT('Ctrl Pts',(13.4060235269164,0.0475779130258999,
4.59111527567571));
#14279=CARTESIAN_POINT('Ctrl Pts',(13.4296376430663,-0.238699550200797,
4.5428659610613));
#14280=CARTESIAN_POINT('Ctrl Pts',(13.4532517592162,-0.467771004553565,
4.36451503980497));
#14281=CARTESIAN_POINT('Ctrl Pts',(13.476865875366,-0.584737881352888,4.09880555174689));
#14282=CARTESIAN_POINT('Ctrl Pts',(13.5004799915159,-0.561568254327815,
3.80941662539381));
#14283=CARTESIAN_POINT('Ctrl Pts',(13.5240941076658,-0.403814885886516,
3.56570233148043));
#14284=CARTESIAN_POINT('Ctrl Pts',(13.5477082238157,-0.149284468950505,
3.42607049712074));
#14285=CARTESIAN_POINT('Ctrl Pts',(13.5713223399655,0.141023010189178,3.42398486344345));
#14286=CARTESIAN_POINT('Ctrl Pts',(13.5949364561154,0.39753334322815,3.55994526707815));
#14287=CARTESIAN_POINT('Ctrl Pts',(13.6185505722652,0.55877204319843,3.8013678508274));
#14288=CARTESIAN_POINT('Ctrl Pts',(13.6421646884151,0.586097133215014,4.09039401187145));
#14289=CARTESIAN_POINT('Ctrl Pts',(13.665778804565,0.47295996523623,4.35775661870721));
#14290=CARTESIAN_POINT('Ctrl Pts',(13.6893929207148,0.24647464915429,4.53938036140496));
#14291=CARTESIAN_POINT('Ctrl Pts',(13.7130070368647,-0.0390800323908759,
4.59173784568287));
#14292=CARTESIAN_POINT('Ctrl Pts',(13.7366211530146,-0.315268912124245,
4.50228123595558));
#14293=CARTESIAN_POINT('Ctrl Pts',(13.7602352691644,-0.515901402373503,
4.29244943148197));
#14294=CARTESIAN_POINT('Ctrl Pts',(13.7838493853143,-0.59289453017979,4.01253008491428));
#14295=CARTESIAN_POINT('Ctrl Pts',(13.8074635014642,-0.527796356489121,
3.72960781627073));
#14296=CARTESIAN_POINT('Ctrl Pts',(13.831077617614,-0.336208111796874,3.51148691674935));
#14297=CARTESIAN_POINT('Ctrl Pts',(13.8546917337639,-0.0640452526541193,
3.4104415783338));
#14298=CARTESIAN_POINT('Ctrl Pts',(13.8783058499138,0.223466497127862,3.45068801978614));
#14299=CARTESIAN_POINT('Ctrl Pts',(13.9019199660636,0.457422945247278,3.62258090124322));
#14300=CARTESIAN_POINT('Ctrl Pts',(13.9255340822135,0.581754800262342,3.88492489705937));
#14301=CARTESIAN_POINT('Ctrl Pts',(13.9491481983634,0.566665067602596,4.17484744237197));
#14302=CARTESIAN_POINT('Ctrl Pts',(13.9727623145132,0.415770106744681,4.42286658094793));
#14303=CARTESIAN_POINT('Ctrl Pts',(13.9963764306631,0.165232945489059,4.56954279968241));
#14304=CARTESIAN_POINT('Ctrl Pts',(14.019990546813,-0.124903441395439,4.57972412169294));
#14305=CARTESIAN_POINT('Ctrl Pts',(14.0436046629628,-0.385105849054417,
4.45097052228405));
#14306=CARTESIAN_POINT('Ctrl Pts',(14.0672187791127,-0.553014959135429,
4.21413869785145));
#14307=CARTESIAN_POINT('Ctrl Pts',(14.0908328952626,-0.58839018453545,3.92598704378684));
#14308=CARTESIAN_POINT('Ctrl Pts',(14.1144470114124,-0.482753606228458,
3.65557310990793));
#14309=CARTESIAN_POINT('Ctrl Pts',(14.1380611275623,-0.261421765577673,
3.46770347791168));
#14310=CARTESIAN_POINT('Ctrl Pts',(14.1616752437122,0.0225616210391343,
3.40740241293002));
#14311=CARTESIAN_POINT('Ctrl Pts',(14.185289359862,0.301137958114838,3.48912148496193));
#14312=CARTESIAN_POINT('Ctrl Pts',(14.2089034760119,0.507544487205137,3.69327614952086));
#14313=CARTESIAN_POINT('Ctrl Pts',(14.2325175921618,0.592314446747875,3.97093932005559));
#14314=CARTESIAN_POINT('Ctrl Pts',(14.2561317083116,0.535132125826274,4.25556708484021));
#14315=CARTESIAN_POINT('Ctrl Pts',(14.2797458244615,0.349701665714674,4.47894641865396));
#14316=CARTESIAN_POINT('Ctrl Pts',(14.3033599406114,0.0804627670229728,
4.58754290912926));
#14317=CARTESIAN_POINT('Ctrl Pts',(14.3269740567612,-0.208059593914322,
4.55533065134682));
#14318=CARTESIAN_POINT('Ctrl Pts',(14.3505881729111,-0.44671902479684,4.39002953712461));
#14319=CARTESIAN_POINT('Ctrl Pts',(14.374202289061,-0.578319131624566,4.13125512920294));
#14320=CARTESIAN_POINT('Ctrl Pts',(14.3978164052108,-0.571321032683373,
3.84102451585645));
#14321=CARTESIAN_POINT('Ctrl Pts',(14.4214305213607,-0.427401871100662,
3.58889348396707));
#14322=CARTESIAN_POINT('Ctrl Pts',(14.4450446375106,-0.181052875819672,
3.43528699049651));
#14323=CARTESIAN_POINT('Ctrl Pts',(14.4686587536604,0.108686701521778,3.41701790091169));
#14324=CARTESIAN_POINT('Ctrl Pts',(14.4922728698103,0.372378754238714,3.53846452970905));
#14325=CARTESIAN_POINT('Ctrl Pts',(14.5158869859602,0.546827646247725,3.77052134686598));
#14326=CARTESIAN_POINT('Ctrl Pts',(14.53950110211,0.59022548618159,4.05757432072539));
#14327=CARTESIAN_POINT('Ctrl Pts',(14.5631152182599,0.492171679592087,4.3308292078278));
#14328=CARTESIAN_POINT('Ctrl Pts',(14.5867293344098,0.276165503816305,4.52479857226205));
#14329=CARTESIAN_POINT('Ctrl Pts',(14.6103434505596,-0.00602565743375084,
4.59299630554951));
#14330=CARTESIAN_POINT('Ctrl Pts',(14.6339575667095,-0.286772727926288,
4.51907834617235));
#14331=CARTESIAN_POINT('Ctrl Pts',(14.6575716828594,-0.49879271786407,4.32075964763751));
#14332=CARTESIAN_POINT('Ctrl Pts',(14.6811857990092,-0.591273560669336,
4.04556866666751));
#14333=CARTESIAN_POINT('Ctrl Pts',(14.7047999151591,-0.542051578672567,
3.75945683743125));
#14334=CARTESIAN_POINT('Ctrl Pts',(14.728414031309,-0.362923162297683,3.53099285177933));
#14335=CARTESIAN_POINT('Ctrl Pts',(14.7520281474588,-0.0968176839575538,
3.41492969374656));
#14336=CARTESIAN_POINT('Ctrl Pts',(14.7756422636087,0.192490826988301,3.43908270827084));
#14337=CARTESIAN_POINT('Ctrl Pts',(14.7992563797586,0.435667569828913,3.59766345479839));
#14338=CARTESIAN_POINT('Ctrl Pts',(14.8228704959084,0.574433549780463,3.85266695881428));
#14339=CARTESIAN_POINT('Ctrl Pts',(14.8464846120583,0.575532524168,4.14297984400973));
#14340=CARTESIAN_POINT('Ctrl Pts',(14.8700987282082,0.438701136655627,4.39902663091346));
#14341=CARTESIAN_POINT('Ctrl Pts',(14.893712844358,0.196731937819222,4.55944387228049));
#14342=CARTESIAN_POINT('Ctrl Pts',(14.9173269605079,-0.0923853752310475,
4.58578657160514));
#14343=CARTESIAN_POINT('Ctrl Pts',(14.9409410766578,-0.359362027571537,
4.47174127747511));
#14344=CARTESIAN_POINT('Ctrl Pts',(14.9645551928076,-0.540214773976066,
4.24464025294543));
#14345=CARTESIAN_POINT('Ctrl Pts',(14.9881693089575,-0.59160192159185,3.95890873763601));
#14346=CARTESIAN_POINT('Ctrl Pts',(15.0117834251074,-0.501206205285789,
3.68302663884805));
#14347=CARTESIAN_POINT('Ctrl Pts',(15.0353975412572,-0.290695865081771,
3.48310596742652));
#14348=CARTESIAN_POINT('Ctrl Pts',(15.0590116574071,-0.0105122258222001,
3.40706994202017));
#14349=CARTESIAN_POINT('Ctrl Pts',(15.082625773557,0.272176412698783,3.47311795657709));
#14350=CARTESIAN_POINT('Ctrl Pts',(15.1062398897068,0.489659512974156,3.66547122397039));
#14351=CARTESIAN_POINT('Ctrl Pts',(15.1219826338067,0.5563490739778,3.84710486709154));
#14352=CARTESIAN_POINT('Ctrl Pts',(15.1298540058567,0.566167676482186,3.94044192881839));
#14353=CARTESIAN_POINT('Ctrl Pts',(12.4701459941433,0.254789069842909,4.44592641788345));
#14354=CARTESIAN_POINT('Ctrl Pts',(12.4780173661933,0.181274697121691,4.48793034026739));
#14355=CARTESIAN_POINT('Ctrl Pts',(12.4937601102932,0.0131377437512366,
4.53483083224977));
#14356=CARTESIAN_POINT('Ctrl Pts',(12.517374226443,-0.242323003376296,4.47697306011837));
#14357=CARTESIAN_POINT('Ctrl Pts',(12.5409883425929,-0.439671888977142,
4.30480445207012));
#14358=CARTESIAN_POINT('Ctrl Pts',(12.5646024587428,-0.531669448515955,
4.05958515863483));
#14359=CARTESIAN_POINT('Ctrl Pts',(12.5882165748926,-0.496240142441994,
3.80008637217214));
#14360=CARTESIAN_POINT('Ctrl Pts',(12.6118306910425,-0.341887499674706,
3.58849794711368));
#14361=CARTESIAN_POINT('Ctrl Pts',(12.6354448071924,-0.105597250297878,
3.47552899021694));
#14362=CARTESIAN_POINT('Ctrl Pts',(12.6590589233422,0.155999231932725,3.4882530946792));
#14363=CARTESIAN_POINT('Ctrl Pts',(12.6826730394921,0.380209824197002,3.62362093815591));
#14364=CARTESIAN_POINT('Ctrl Pts',(12.706287155642,0.513300292941022,3.84919062944795));
#14365=CARTESIAN_POINT('Ctrl Pts',(12.7299012717918,0.52337486302099,4.11090284295443));
#14366=CARTESIAN_POINT('Ctrl Pts',(12.7535153879417,0.408018961865605,4.34603641497018));
#14367=CARTESIAN_POINT('Ctrl Pts',(12.7771295040916,0.194878495711741,4.49823995272895));
#14368=CARTESIAN_POINT('Ctrl Pts',(12.8007436202414,-0.0649659676909401,
4.53103681671432));
#14369=CARTESIAN_POINT('Ctrl Pts',(12.8243577363913,-0.30924088042124,4.43656701116699));
#14370=CARTESIAN_POINT('Ctrl Pts',(12.8479718525412,-0.479404065419363,
4.23747088215356));
#14371=CARTESIAN_POINT('Ctrl Pts',(12.871585968691,-0.534674727916345,3.9814632031866));
#14372=CARTESIAN_POINT('Ctrl Pts',(12.8952000848409,-0.461806870250484,
3.72989799658434));
#14373=CARTESIAN_POINT('Ctrl Pts',(12.9188142009908,-0.278263781132688,
3.54306461538724));
#14374=CARTESIAN_POINT('Ctrl Pts',(12.9424283171406,-0.0280328398727138,
3.46573897998727));
#14375=CARTESIAN_POINT('Ctrl Pts',(12.9660424332905,0.228916366652986,3.51645271720832));
#14376=CARTESIAN_POINT('Ctrl Pts',(12.9896565494404,0.431004172325429,3.68305192688505));
#14377=CARTESIAN_POINT('Ctrl Pts',(13.0132706655902,0.529798827743877,3.92560994866724));
#14378=CARTESIAN_POINT('Ctrl Pts',(13.0368847817401,0.501623505980173,4.1859960641053));
#14379=CARTESIAN_POINT('Ctrl Pts',(13.06049889789,0.353230619039521,4.40180692799916));
#14380=CARTESIAN_POINT('Ctrl Pts',(13.0841130140398,0.120183555287252,4.52132196448402));
#14381=CARTESIAN_POINT('Ctrl Pts',(13.1077271301897,-0.14166633412753,4.51589856308179));
#14382=CARTESIAN_POINT('Ctrl Pts',(13.1313412463396,-0.369564900381594,
4.38683647969259));
#14383=CARTESIAN_POINT('Ctrl Pts',(13.1549553624894,-0.508894665592834,
4.16506634104549));
#14384=CARTESIAN_POINT('Ctrl Pts',(13.1785694786393,-0.5262642816069,3.9037369046842));
#14385=CARTESIAN_POINT('Ctrl Pts',(13.2021835947892,-0.417510999030181,
3.66547758923531));
#14386=CARTESIAN_POINT('Ctrl Pts',(13.225797710939,-0.208698299100604,3.50738889824983));
#14387=CARTESIAN_POINT('Ctrl Pts',(13.2494118270889,0.0501304010278875,
3.46735788703128));
#14388=CARTESIAN_POINT('Ctrl Pts',(13.2730259432388,0.296945001575366,3.55497826608759));
#14389=CARTESIAN_POINT('Ctrl Pts',(13.2966400593886,0.472594665360713,3.74925120162283));
#14390=CARTESIAN_POINT('Ctrl Pts',(13.3202541755385,0.534983727701048,4.00361783223636));
#14391=CARTESIAN_POINT('Ctrl Pts',(13.3438682916884,0.469160215495142,4.25711742416948));
#14392=CARTESIAN_POINT('Ctrl Pts',(13.3674824078382,0.290899191662876,4.44899703551904));
#14393=CARTESIAN_POINT('Ctrl Pts',(13.3910965239881,0.0429221515009326,
4.53327138168622));
#14394=CARTESIAN_POINT('Ctrl Pts',(13.414710640138,-0.215341481063824,4.48974352894983));
#14395=CARTESIAN_POINT('Ctrl Pts',(13.4383247562878,-0.421997028626747,
4.32884523023027));
#14396=CARTESIAN_POINT('Ctrl Pts',(13.4619388724377,-0.527518050615216,
4.08913688288313));
#14397=CARTESIAN_POINT('Ctrl Pts',(13.4855529885876,-0.506615699542168,
3.82806626104107));
#14398=CARTESIAN_POINT('Ctrl Pts',(13.5091671047374,-0.364299369350597,
3.60820075662942));
#14399=CARTESIAN_POINT('Ctrl Pts',(13.5327812208873,-0.134676159283021,
3.48223266833859));
#14400=CARTESIAN_POINT('Ctrl Pts',(13.5563953370372,0.127223129883027,3.48035112543394));
#14401=CARTESIAN_POINT('Ctrl Pts',(13.580009453187,0.35863251032937,3.60300705277064));
#14402=CARTESIAN_POINT('Ctrl Pts',(13.6036235693369,0.504093113113068,3.82080510351303));
#14403=CARTESIAN_POINT('Ctrl Pts',(13.6272376854868,0.528744292176554,4.08154845863482));
#14404=CARTESIAN_POINT('Ctrl Pts',(13.6508518016366,0.426678220852065,4.32274815795836));
#14405=CARTESIAN_POINT('Ctrl Pts',(13.6744659177865,0.222355743648963,4.48659901446809));
#14406=CARTESIAN_POINT('Ctrl Pts',(13.6980800339364,-0.0352558354131549,
4.53383302978021));
#14407=CARTESIAN_POINT('Ctrl Pts',(13.7216941500862,-0.284418108090716,
4.45313024331322));
#14408=CARTESIAN_POINT('Ctrl Pts',(13.7453082662361,-0.465417601233682,
4.26383163964332));
#14409=CARTESIAN_POINT('Ctrl Pts',(13.768922382386,-0.534876526311652,4.01130394691162));
#14410=CARTESIAN_POINT('Ctrl Pts',(13.7925364985358,-0.476148568402614,
3.75606718461195));
#14411=CARTESIAN_POINT('Ctrl Pts',(13.8161506146857,-0.303308291444651,
3.55929061961886));
#14412=CARTESIAN_POINT('Ctrl Pts',(13.8397647308356,-0.0577780710103693,
3.46813312556118));
#14413=CARTESIAN_POINT('Ctrl Pts',(13.8633788469854,0.201599066354243,3.50444123046797));
#14414=CARTESIAN_POINT('Ctrl Pts',(13.8869929631353,0.412661584067771,3.65951344424533));
#14415=CARTESIAN_POINT('Ctrl Pts',(13.9106070792852,0.52482688048259,3.89618563135138));
#14416=CARTESIAN_POINT('Ctrl Pts',(13.934221195435,0.511213761492322,4.157737654591));
#14417=CARTESIAN_POINT('Ctrl Pts',(13.9578353115849,0.375084705828511,4.38148675084272));
#14418=CARTESIAN_POINT('Ctrl Pts',(13.9814494277348,0.149063989321389,4.51380989159668));
#14419=CARTESIAN_POINT('Ctrl Pts',(14.0050635438846,-0.112680949911453,
4.52299491502504));
#14420=CARTESIAN_POINT('Ctrl Pts',(14.0286776600345,-0.347421115087809,
4.40684056632315));
#14421=CARTESIAN_POINT('Ctrl Pts',(14.0522917761844,-0.498899391517477,
4.19318404374712));
#14422=CARTESIAN_POINT('Ctrl Pts',(14.0759058923342,-0.530812955762567,
3.93322962026762));
#14423=CARTESIAN_POINT('Ctrl Pts',(14.0995200084841,-0.435513499990629,
3.68927718310219));
#14424=CARTESIAN_POINT('Ctrl Pts',(14.123134124634,-0.235840202189154,3.51979163205294));
#14425=CARTESIAN_POINT('Ctrl Pts',(14.1467482407838,0.020353841830372,3.46539135927508));
#14426=CARTESIAN_POINT('Ctrl Pts',(14.1703623569337,0.271669945965271,3.53911376883853));
#14427=CARTESIAN_POINT('Ctrl Pts',(14.1939764730836,0.457878456363209,3.72329077208477));
#14428=CARTESIAN_POINT('Ctrl Pts',(14.2175905892334,0.534353207246894,3.97378306806742));
#14429=CARTESIAN_POINT('Ctrl Pts',(14.2412047053833,0.482766492200443,4.23055843429265));
#14430=CARTESIAN_POINT('Ctrl Pts',(14.2648188215332,0.315481426597312,4.4320788667444));
#14431=CARTESIAN_POINT('Ctrl Pts',(14.288432937683,0.0725890409372144,4.53004859093371));
#14432=CARTESIAN_POINT('Ctrl Pts',(14.3120470538329,-0.187699813700353,
4.50098848045824));
#14433=CARTESIAN_POINT('Ctrl Pts',(14.3356611699828,-0.40300510134274,4.35186299309067));
#14434=CARTESIAN_POINT('Ctrl Pts',(14.3592752861326,-0.521727410993515,
4.11841108999162));
#14435=CARTESIAN_POINT('Ctrl Pts',(14.3828894022825,-0.515414114678713,
3.85658114487643));
#14436=CARTESIAN_POINT('Ctrl Pts',(14.4065035184324,-0.385578237809175,
3.62912252677875));
#14437=CARTESIAN_POINT('Ctrl Pts',(14.4301176345822,-0.163335852108122,
3.49054727694211));
#14438=CARTESIAN_POINT('Ctrl Pts',(14.4537317507321,0.0980511075867261,
3.47406591865897));
#14439=CARTESIAN_POINT('Ctrl Pts',(14.477345866882,0.335939436781555,3.58362832417432));
#14440=CARTESIAN_POINT('Ctrl Pts',(14.5009599830318,0.493317541363497,3.79297710030521));
#14441=CARTESIAN_POINT('Ctrl Pts',(14.5245740991817,0.532468663007706,4.05194035550473));
#14442=CARTESIAN_POINT('Ctrl Pts',(14.5481882153316,0.444009962867018,4.2984557429324));
#14443=CARTESIAN_POINT('Ctrl Pts',(14.5718023314814,0.249141184223067,4.47344413391656));
#14444=CARTESIAN_POINT('Ctrl Pts',(14.5954164476313,-0.00543601357889273,
4.53496834239941));
#14445=CARTESIAN_POINT('Ctrl Pts',(14.6190305637812,-0.258710432878536,
4.46828366353805));
#14446=CARTESIAN_POINT('Ctrl Pts',(14.642644679931,-0.449983095981302,4.28937154481299));
#14447=CARTESIAN_POINT('Ctrl Pts',(14.6662587960809,-0.533414177619135,
4.0411095209942));
#14448=CARTESIAN_POINT('Ctrl Pts',(14.6898729122308,-0.489008838375032,
3.78299531421925));
#14449=CARTESIAN_POINT('Ctrl Pts',(14.7134870283806,-0.327409126727749,
3.57688779119022));
#14450=CARTESIAN_POINT('Ctrl Pts',(14.7371011445305,-0.0873435389344073,
3.47218205409647));
#14451=CARTESIAN_POINT('Ctrl Pts',(14.7607152606804,0.173654536592096,3.49397156277145));
#14452=CARTESIAN_POINT('Ctrl Pts',(14.7843293768302,0.393035092271916,3.63703430753458));
#14453=CARTESIAN_POINT('Ctrl Pts',(14.8079434929801,0.518222054789869,3.86708431049878));
#14454=CARTESIAN_POINT('Ctrl Pts',(14.8315576091299,0.519213488464815,4.12898847670818));
#14455=CARTESIAN_POINT('Ctrl Pts',(14.8551717252798,0.395771807832633,4.35997967156842));
#14456=CARTESIAN_POINT('Ctrl Pts',(14.8787858414297,0.177480631307892,4.50469920000947));
#14457=CARTESIAN_POINT('Ctrl Pts',(14.9023999575796,-0.0833449560929437,
4.52846412073519));
#14458=CARTESIAN_POINT('Ctrl Pts',(14.9260140737294,-0.324196468699902,
4.42557878841823));
#14459=CARTESIAN_POINT('Ctrl Pts',(14.9496281898793,-0.487351775161311,
4.22070085323907));
#14460=CARTESIAN_POINT('Ctrl Pts',(14.9732423060292,-0.533710406612102,
3.96292974457304));
#14461=CARTESIAN_POINT('Ctrl Pts',(14.996856422179,-0.452160410331013,3.71404423263127));
#14462=CARTESIAN_POINT('Ctrl Pts',(15.0204705383289,-0.262249669398955,
3.53368690291293));
#14463=CARTESIAN_POINT('Ctrl Pts',(15.0440846544788,-0.0094835464747447,
3.46509142247974));
#14464=CARTESIAN_POINT('Ctrl Pts',(15.0676987706286,0.245542447700007,3.52467627408104));
#14465=CARTESIAN_POINT('Ctrl Pts',(15.0913128867785,0.441743625625371,3.69820671204414));
#14466=CARTESIAN_POINT('Ctrl Pts',(15.1070556308784,0.501907244810829,3.86206650016617));
#14467=CARTESIAN_POINT('Ctrl Pts',(15.1149270029284,0.510765042839744,3.94627001497588));
#14468=CARTESIAN_POINT('Ctrl Pts',(12.4552189912149,0.227152124655503,4.39755682347243));
#14469=CARTESIAN_POINT('Ctrl Pts',(12.4630903632649,0.161611848667067,4.43500458455284));
#14470=CARTESIAN_POINT('Ctrl Pts',(12.4788331073648,0.0117126939868845,
4.476817784812));
#14471=CARTESIAN_POINT('Ctrl Pts',(12.5024472235147,-0.216038251184659,
4.42523583949706));
#14472=CARTESIAN_POINT('Ctrl Pts',(12.5260613396645,-0.391980722697534,
4.27174234332294));
#14473=CARTESIAN_POINT('Ctrl Pts',(12.5496754558144,-0.473999316058885,
4.05312196237532));
#14474=CARTESIAN_POINT('Ctrl Pts',(12.5732895719643,-0.442413023308054,
3.82177098359562));
#14475=CARTESIAN_POINT('Ctrl Pts',(12.5969036881141,-0.304802996424253,
3.6331335340607));
#14476=CARTESIAN_POINT('Ctrl Pts',(12.620517804264,-0.0941431270098475,
3.53241830873714));
#14477=CARTESIAN_POINT('Ctrl Pts',(12.6441319204139,0.139078010685439,3.54376223084778));
#14478=CARTESIAN_POINT('Ctrl Pts',(12.6677460365637,0.338968502198674,3.66444673774097));
#14479=CARTESIAN_POINT('Ctrl Pts',(12.6913601527136,0.457622660971028,3.86554890694496));
#14480=CARTESIAN_POINT('Ctrl Pts',(12.7149742688635,0.46660444343158,4.09887322255608));
#14481=CARTESIAN_POINT('Ctrl Pts',(12.7385883850133,0.36376118545685,4.30850187928827));
#14482=CARTESIAN_POINT('Ctrl Pts',(12.7622025011632,0.173740044570527,4.44419591437112));
#14483=CARTESIAN_POINT('Ctrl Pts',(12.7858166173131,-0.0579191156056905,
4.47343530576616));
#14484=CARTESIAN_POINT('Ctrl Pts',(12.809430733463,-0.275697552729921,4.38921263067613));
#14485=CARTESIAN_POINT('Ctrl Pts',(12.8330448496128,-0.42740315389367,4.2117124390707));
#14486=CARTESIAN_POINT('Ctrl Pts',(12.8566589657627,-0.476678613100171,
3.98347388770222));
#14487=CARTESIAN_POINT('Ctrl Pts',(12.8802730819125,-0.411714724743029,
3.75919593416074));
#14488=CARTESIAN_POINT('Ctrl Pts',(12.9038871980624,-0.248080536335154,
3.59262835132974));
#14489=CARTESIAN_POINT('Ctrl Pts',(12.9275013142123,-0.0249921205063485,
3.52369021994808));
#14490=CARTESIAN_POINT('Ctrl Pts',(12.9511154303621,0.204085831019768,3.5689030431123));
#14491=CARTESIAN_POINT('Ctrl Pts',(12.974729546512,0.384253192413122,3.71743125300502));
#14492=CARTESIAN_POINT('Ctrl Pts',(12.9983436626619,0.472331601336806,3.93367903017235));
#14493=CARTESIAN_POINT('Ctrl Pts',(13.0219577788117,0.44721245393608,4.16582108944128));
#14494=CARTESIAN_POINT('Ctrl Pts',(13.0455718949616,0.314915728754283,4.35822297028905));
#14495=CARTESIAN_POINT('Ctrl Pts',(13.0691860111115,0.107147256940744,4.46477422259573));
#14496=CARTESIAN_POINT('Ctrl Pts',(13.0928001272613,-0.126299800886535,
4.4599390970068));
#14497=CARTESIAN_POINT('Ctrl Pts',(13.1164142434112,-0.329478232215912,
4.34487636502855));
#14498=CARTESIAN_POINT('Ctrl Pts',(13.1400283595611,-0.453694911585238,
4.14716161137019));
#14499=CARTESIAN_POINT('Ctrl Pts',(13.1636424757109,-0.469180447069464,
3.9141785531052));
#14500=CARTESIAN_POINT('Ctrl Pts',(13.1872565918608,-0.372223622289685,
3.70176320202068));
#14501=CARTESIAN_POINT('Ctrl Pts',(13.2108707080107,-0.186060815253654,
3.56082237569912));
#14502=CARTESIAN_POINT('Ctrl Pts',(13.2344848241605,0.0446927613901878,
3.52513352430527));
#14503=CARTESIAN_POINT('Ctrl Pts',(13.2580989403104,0.26473540664544,3.60324972951781));
#14504=CARTESIAN_POINT('Ctrl Pts',(13.2817130564603,0.421332368785403,3.77644989896424));
#14505=CARTESIAN_POINT('Ctrl Pts',(13.3053271726101,0.476954095708811,4.00322540633176));
#14506=CARTESIAN_POINT('Ctrl Pts',(13.32894128876,0.418270453356816,4.22922792261873));
#14507=CARTESIAN_POINT('Ctrl Pts',(13.3525554049099,0.259345385135757,4.40029437151701));
#14508=CARTESIAN_POINT('Ctrl Pts',(13.3761695210597,0.0382663899759653,
4.47542748769673));
#14509=CARTESIAN_POINT('Ctrl Pts',(13.3997836372096,-0.19198341192685,4.43662109683837));
#14510=CARTESIAN_POINT('Ctrl Pts',(13.4233977533595,-0.376223052699929,
4.29317542065556));
#14511=CARTESIAN_POINT('Ctrl Pts',(13.4470118695093,-0.470298219877544,
4.07946821401937));
#14512=CARTESIAN_POINT('Ctrl Pts',(13.4706259856592,-0.451663144756522,
3.84671589668833));
#14513=CARTESIAN_POINT('Ctrl Pts',(13.4942401018091,-0.324783852814677,
3.65069918177841));
#14514=CARTESIAN_POINT('Ctrl Pts',(13.5178542179589,-0.120067849615538,
3.53839483955645));
#14515=CARTESIAN_POINT('Ctrl Pts',(13.5414683341088,0.113423249576877,3.53671738742444));
#14516=CARTESIAN_POINT('Ctrl Pts',(13.5650824502587,0.319731677430589,3.64606883846313));
#14517=CARTESIAN_POINT('Ctrl Pts',(13.5886965664085,0.449414183027706,3.84024235619866));
#14518=CARTESIAN_POINT('Ctrl Pts',(13.6123106825584,0.471391451138094,4.07270290539818));
#14519=CARTESIAN_POINT('Ctrl Pts',(13.6359247987083,0.380396476467901,4.28773969720951));
#14520=CARTESIAN_POINT('Ctrl Pts',(13.6595389148581,0.198236838143636,4.43381766753122));
#14521=CARTESIAN_POINT('Ctrl Pts',(13.683153031008,-0.0314316384354341,
4.47592821387755));
#14522=CARTESIAN_POINT('Ctrl Pts',(13.7067671471579,-0.253567304057185,
4.40397925067086));
#14523=CARTESIAN_POINT('Ctrl Pts',(13.7303812633077,-0.414933800093862,
4.23521384780468));
#14524=CARTESIAN_POINT('Ctrl Pts',(13.7539953794576,-0.476858522443512,
4.01007780890896));
#14525=CARTESIAN_POINT('Ctrl Pts',(13.7776094956075,-0.424500780316106,
3.78252655295316));
#14526=CARTESIAN_POINT('Ctrl Pts',(13.8012236117573,-0.270408471092428,
3.60709432248837));
#14527=CARTESIAN_POINT('Ctrl Pts',(13.8248377279072,-0.0515108893666192,
3.52582467278856));
#14528=CARTESIAN_POINT('Ctrl Pts',(13.8484518440571,0.179731635580624,3.55819444114981));
#14529=CARTESIAN_POINT('Ctrl Pts',(13.8720659602069,0.367900222888263,3.69644598724744));
#14530=CARTESIAN_POINT('Ctrl Pts',(13.8956800763568,0.467898960702838,3.90744636564338));
#14531=CARTESIAN_POINT('Ctrl Pts',(13.9192941925067,0.455762455382048,4.14062786681004));
#14532=CARTESIAN_POINT('Ctrl Pts',(13.9429083086565,0.33439930491234,4.34010692073752));
#14533=CARTESIAN_POINT('Ctrl Pts',(13.9665224248064,0.132895033153719,4.45807698351094));
#14534=CARTESIAN_POINT('Ctrl Pts',(13.9901365409563,-0.100458458427467,
4.46626570835715));
#14535=CARTESIAN_POINT('Ctrl Pts',(14.0137506571061,-0.309736381121202,
4.36271061036225));
#14536=CARTESIAN_POINT('Ctrl Pts',(14.037364773256,-0.444783823899526,4.1722293896428));
#14537=CARTESIAN_POINT('Ctrl Pts',(14.0609788894059,-0.473235726989685,
3.94047219674841));
#14538=CARTESIAN_POINT('Ctrl Pts',(14.0845930055557,-0.388273393752801,
3.72298125629644));
#14539=CARTESIAN_POINT('Ctrl Pts',(14.1082071217056,-0.210258638800633,
3.5718797861942));
#14540=CARTESIAN_POINT('Ctrl Pts',(14.1318212378555,0.0181460626216094,
3.52338030562014));
#14541=CARTESIAN_POINT('Ctrl Pts',(14.1554353540053,0.242201933815703,3.58910605271512));
#14542=CARTESIAN_POINT('Ctrl Pts',(14.1790494701552,0.40821242552128,3.75330539464867));
#14543=CARTESIAN_POINT('Ctrl Pts',(14.2026635863051,0.476391967745912,3.97662681607925));
#14544=CARTESIAN_POINT('Ctrl Pts',(14.2262777024549,0.430400858574612,4.20554978374509));
#14545=CARTESIAN_POINT('Ctrl Pts',(14.2498918186048,0.28126118747995,4.38521131483484));
#14546=CARTESIAN_POINT('Ctrl Pts',(14.2735059347547,0.0647153148514563,
4.47255427273816));
#14547=CARTESIAN_POINT('Ctrl Pts',(14.2971200509045,-0.167340033486385,
4.44664630956965));
#14548=CARTESIAN_POINT('Ctrl Pts',(14.3207341670544,-0.359291177888639,
4.31369644905674));
#14549=CARTESIAN_POINT('Ctrl Pts',(14.3443482832043,-0.465135690362464,
4.10556705078029));
#14550=CARTESIAN_POINT('Ctrl Pts',(14.3679623993541,-0.459507196674052,
3.87213777389641));
#14551=CARTESIAN_POINT('Ctrl Pts',(14.391576515504,-0.343754604517688,3.66935156959044));
#14552=CARTESIAN_POINT('Ctrl Pts',(14.4151906316539,-0.145618828396573,
3.5458075633877));
#14553=CARTESIAN_POINT('Ctrl Pts',(14.4388047478037,0.0874155136516737,
3.53111393640625));
#14554=CARTESIAN_POINT('Ctrl Pts',(14.4624188639536,0.299500119324396,3.6287921186396));
#14555=CARTESIAN_POINT('Ctrl Pts',(14.4860329801035,0.439807436479269,3.81543285374444));
#14556=CARTESIAN_POINT('Ctrl Pts',(14.5096470962533,0.474711839833821,4.04630639028407));
#14557=CARTESIAN_POINT('Ctrl Pts',(14.5332612124032,0.395848246141948,4.26608227803701));
#14558=CARTESIAN_POINT('Ctrl Pts',(14.5568753285531,0.22211686462983,4.42208969557108));
#14559=CARTESIAN_POINT('Ctrl Pts',(14.5804894447029,-0.00484636972403486,
4.47694037924932));
#14560=CARTESIAN_POINT('Ctrl Pts',(14.6041035608528,-0.230648137830783,
4.41748898090375));
#14561=CARTESIAN_POINT('Ctrl Pts',(14.6277176770027,-0.401173474098533,
4.25798344198848));
#14562=CARTESIAN_POINT('Ctrl Pts',(14.6513317931525,-0.475554794568933,
4.03665037532088));
#14563=CARTESIAN_POINT('Ctrl Pts',(14.6749459093024,-0.435966098077497,
3.80653379100725));
#14564=CARTESIAN_POINT('Ctrl Pts',(14.6985600254523,-0.291895091157815,
3.62278273060111));
#14565=CARTESIAN_POINT('Ctrl Pts',(14.7221741416021,-0.077869393911261,
3.52943441444639));
#14566=CARTESIAN_POINT('Ctrl Pts',(14.745788257752,0.15481824619589,3.54886041727207));
#14567=CARTESIAN_POINT('Ctrl Pts',(14.7694023739019,0.350402614714918,3.67640516027076));
#14568=CARTESIAN_POINT('Ctrl Pts',(14.7930164900517,0.462010559799276,3.88150166218328));
#14569=CARTESIAN_POINT('Ctrl Pts',(14.8166306062016,0.46289445276163,4.11499710940664));
#14570=CARTESIAN_POINT('Ctrl Pts',(14.8402447223515,0.352842479009638,4.32093271222338));
#14571=CARTESIAN_POINT('Ctrl Pts',(14.8638588385013,0.158229324796562,4.44995452773844));
#14572=CARTESIAN_POINT('Ctrl Pts',(14.8874729546512,-0.07430453695484,4.47114166986524));
#14573=CARTESIAN_POINT('Ctrl Pts',(14.9110870708011,-0.289030909828268,
4.37941629936134));
#14574=CARTESIAN_POINT('Ctrl Pts',(14.9347011869509,-0.434488776346555,
4.1967614535327));
#14575=CARTESIAN_POINT('Ctrl Pts',(14.9583153031008,-0.475818891632353,
3.96695075151007));
#14576=CARTESIAN_POINT('Ctrl Pts',(14.9819294192507,-0.403114615376237,
3.74506182641449));
#14577=CARTESIAN_POINT('Ctrl Pts',(15.0055435354005,-0.233803473716137,
3.58426783839933));
#14578=CARTESIAN_POINT('Ctrl Pts',(15.0291576515504,-0.00845486712728951,
3.5231129029393));
#14579=CARTESIAN_POINT('Ctrl Pts',(15.0527717677003,0.218908482701231,3.57623459158499));
#14580=CARTESIAN_POINT('Ctrl Pts',(15.0763858838501,0.393827738276586,3.73094220011788));
#14581=CARTESIAN_POINT('Ctrl Pts',(15.09212862795,0.447465415643859,3.87702813324079));
#14582=CARTESIAN_POINT('Ctrl Pts',(15.1,0.455362409197302,3.95209810113337));
#14583=CARTESIAN_POINT('',(15.1,0.455362409197302,3.95209810113338));
#14584=CARTESIAN_POINT('Ctrl Pts',(15.1,0.455362409197302,3.95209810113337));
#14585=CARTESIAN_POINT('Ctrl Pts',(15.1,0.461198486074795,3.93070554260298));
#14586=CARTESIAN_POINT('Ctrl Pts',(15.1,0.46535922191849,3.9089149747703));
#14587=CARTESIAN_POINT('Ctrl Pts',(15.1,0.467933495509747,3.88694781877637));
#14588=CARTESIAN_POINT('Ctrl Pts',(15.1,0.470556099470815,3.86456824322593));
#14589=CARTESIAN_POINT('Ctrl Pts',(15.1,0.471533159003394,3.84200460508655));
#14590=CARTESIAN_POINT('Ctrl Pts',(15.1,0.470938919222204,3.8194389967166));
#14591=CARTESIAN_POINT('Ctrl Pts',(15.1,0.470570970565677,3.80546654730098));
#14592=CARTESIAN_POINT('Ctrl Pts',(15.1,0.469600118414825,3.7914923521806));
#14593=CARTESIAN_POINT('Ctrl Pts',(15.1,0.468037922355437,3.77755218535593));
#14594=CARTESIAN_POINT('Ctrl Pts',(15.1,0.467305764617198,3.77101881782393));
#14595=CARTESIAN_POINT('Ctrl Pts',(15.1,0.466444065557791,3.76449770946228));
#14596=CARTESIAN_POINT('Ctrl Pts',(15.1,0.465455885979624,3.7580011302485));
#14597=CARTESIAN_POINT('Ctrl Pts',(15.1,0.462059294618766,3.73567095330476));
#14598=CARTESIAN_POINT('Ctrl Pts',(15.1,0.45716703427379,3.71360451488159));
#14599=CARTESIAN_POINT('Ctrl Pts',(15.1,0.450855318277529,3.69195899424001));
#14600=CARTESIAN_POINT('Ctrl Pts',(15.1,0.444011336009419,3.66848810937402));
#14601=CARTESIAN_POINT('Ctrl Pts',(15.1,0.435499564516811,3.64551127788848));
#14602=CARTESIAN_POINT('Ctrl Pts',(15.1,0.425460105602329,3.62314791088594));
#14603=CARTESIAN_POINT('Ctrl Pts',(15.1,0.421555366121865,3.61444992000866));
#14604=CARTESIAN_POINT('Ctrl Pts',(15.1,0.417417266816347,3.60584160863805));
#14605=CARTESIAN_POINT('Ctrl Pts',(15.1,0.413065612826793,3.5973533346642));
#14606=CARTESIAN_POINT('Ctrl Pts',(15.1,0.400188909388694,3.57223622128044));
#14607=CARTESIAN_POINT('Ctrl Pts',(15.1,0.385429835973237,3.54813135585314));
#14608=CARTESIAN_POINT('Ctrl Pts',(15.1,0.369010648251791,3.52520488756047));
#14609=CARTESIAN_POINT('Ctrl Pts',(15.1,0.352591460530346,3.50227841926781));
#14610=CARTESIAN_POINT('Ctrl Pts',(15.1,0.334512091502091,3.48052876229398));
#14611=CARTESIAN_POINT('Ctrl Pts',(15.1,0.31493781544227,3.46010549098216));
#14612=CARTESIAN_POINT('Ctrl Pts',(14.8800042915148,-1.01702808208336E-5,
4.45785711824254));
#14613=CARTESIAN_POINT('Ctrl Pts',(14.8824938458936,-0.0238866377941533,
4.45787702641871));
#14614=CARTESIAN_POINT('Ctrl Pts',(14.8849834002724,-0.0477600743578134,
4.45604121816599));
#14615=CARTESIAN_POINT('Ctrl Pts',(14.8874729546512,-0.0713366221418418,
4.45232291776013));
#14616=CARTESIAN_POINT('Ctrl Pts',(14.8953443267012,-0.145879994579315,
4.44056654636394));
#14617=CARTESIAN_POINT('Ctrl Pts',(14.9032156987511,-0.217455452203791,
4.40999142286264));
#14618=CARTESIAN_POINT('Ctrl Pts',(14.9110870708011,-0.277486158769077,
4.36426138680722));
#14619=CARTESIAN_POINT('Ctrl Pts',(14.918958442851,-0.337516865334364,4.31853135075179));
#14620=CARTESIAN_POINT('Ctrl Pts',(14.926829814901,-0.38600282084046,4.25764640214225));
#14621=CARTESIAN_POINT('Ctrl Pts',(14.9347011869509,-0.417134151141141,
4.18890214416703));
#14622=CARTESIAN_POINT('Ctrl Pts',(14.9425725590009,-0.448265481441821,
4.12015788619182));
#14623=CARTESIAN_POINT('Ctrl Pts',(14.9504439310508,-0.462042186537087,
4.04355431885095));
#14624=CARTESIAN_POINT('Ctrl Pts',(14.9583153031008,-0.456813159708701,
3.96827104766458));
#14625=CARTESIAN_POINT('Ctrl Pts',(14.9661866751508,-0.451584132880315,
3.89298777647821));
#14626=CARTESIAN_POINT('Ctrl Pts',(14.9740580472007,-0.427349374128277,
3.81902480144635));
#14627=CARTESIAN_POINT('Ctrl Pts',(14.9819294192507,-0.387013471142241,
3.7552443159279));
#14628=CARTESIAN_POINT('Ctrl Pts',(14.9898007913006,-0.346677568156205,
3.69146383040944));
#14629=CARTESIAN_POINT('Ctrl Pts',(14.9976721633506,-0.290240520936171,
3.63786583440439));
#14630=CARTESIAN_POINT('Ctrl Pts',(15.0055435354005,-0.224463896228013,
3.60087434715852));
#14631=CARTESIAN_POINT('Ctrl Pts',(15.0134149074505,-0.158687271519854,
3.56388285991266));
#14632=CARTESIAN_POINT('Ctrl Pts',(15.0212862795004,-0.0835710693235713,
3.54349788142598));
#14633=CARTESIAN_POINT('Ctrl Pts',(15.0291576515504,-0.00811907658734153,
3.54215900695692));
#14634=CARTESIAN_POINT('Ctrl Pts',(15.0370290236004,0.067332916148885,3.54082013248786));
#14635=CARTESIAN_POINT('Ctrl Pts',(15.0449003956503,0.143120699425059,3.55852736203643));
#14636=CARTESIAN_POINT('Ctrl Pts',(15.0527717677003,0.210167800325704,3.59316557823286));
#14637=CARTESIAN_POINT('Ctrl Pts',(15.0606431397502,0.27721490122635,3.62780379442929));
#14638=CARTESIAN_POINT('Ctrl Pts',(15.0685145118002,0.335521319751467,3.67937299727358));
#14639=CARTESIAN_POINT('Ctrl Pts',(15.0763858838501,0.378083948355844,3.74167908197646));
#14640=CARTESIAN_POINT('Ctrl Pts',(15.0842572559001,0.420646576960222,3.80398516667934));
#14641=CARTESIAN_POINT('Ctrl Pts',(15.09212862795,0.447465415643859,3.87702813324079));
#14642=CARTESIAN_POINT('Ctrl Pts',(15.1,0.455362409197302,3.95209810113337));
#14643=CARTESIAN_POINT('Ctrl Pts',(12.5,0.310062960217722,4.54266560670548));
#14644=CARTESIAN_POINT('Ctrl Pts',(12.5,0.283442099593322,4.54921865641189));
#14645=CARTESIAN_POINT('Ctrl Pts',(12.5,0.256466577744696,4.55390832200786));
#14646=CARTESIAN_POINT('Ctrl Pts',(12.5,0.229324391633413,4.55669460918752));
#14647=CARTESIAN_POINT('Ctrl Pts',(12.5,0.202804350211112,4.55941702996513));
#14648=CARTESIAN_POINT('Ctrl Pts',(12.5,0.176124140498118,4.56032157710196));
#14649=CARTESIAN_POINT('Ctrl Pts',(12.5,0.149491279718871,4.55933465732487));
#14650=CARTESIAN_POINT('Ctrl Pts',(12.5,0.131604301980395,4.55867182909064));
#14651=CARTESIAN_POINT('Ctrl Pts',(12.5,0.113739373486447,4.5571550748263));
#14652=CARTESIAN_POINT('Ctrl Pts',(12.5,0.0959711573489174,4.5547553284502));
#14653=CARTESIAN_POINT('Ctrl Pts',(12.5,0.0885102514788159,4.55374767063663));
#14654=CARTESIAN_POINT('Ctrl Pts',(12.5,0.0810658284660142,4.55258395860043));
#14655=CARTESIAN_POINT('Ctrl Pts',(12.5,0.0736590895785168,4.55126509319275));
#14656=CARTESIAN_POINT('Ctrl Pts',(12.5,0.0532014046082737,4.54762233847462));
#14657=CARTESIAN_POINT('Ctrl Pts',(12.5,0.0329999615976937,4.54279338637244));
#14658=CARTESIAN_POINT('Ctrl Pts',(12.5,0.0131662989716721,4.53674486487483));
#14659=CARTESIAN_POINT('Ctrl Pts',(12.5,-0.00550403753485725,4.53105111411095));
#14660=CARTESIAN_POINT('Ctrl Pts',(12.5,-0.0238485481480196,4.52427602479051));
#14661=CARTESIAN_POINT('Ctrl Pts',(12.5,-0.0417515783368052,4.51643454453567));
#14662=CARTESIAN_POINT('Ctrl Pts',(12.5,-0.0500477299146631,4.51280085190917));
#14663=CARTESIAN_POINT('Ctrl Pts',(12.5,-0.058248775177811,4.50893813195896));
#14664=CARTESIAN_POINT('Ctrl Pts',(12.5,-0.0663415323109863,4.50484786558969));
#14665=CARTESIAN_POINT('Ctrl Pts',(12.5,-0.0727048112135971,4.50163171746301));
#14666=CARTESIAN_POINT('Ctrl Pts',(12.5,-0.0789919703630761,4.49827952355299));
#14667=CARTESIAN_POINT('Ctrl Pts',(12.5,-0.085197598682301,4.4947927546146));
#14668=CARTESIAN_POINT('Ctrl Pts',(12.5,-0.104491803581693,4.48395188067351));
#14669=CARTESIAN_POINT('Ctrl Pts',(12.5,-0.123002674071495,4.47180959856144));
#14670=CARTESIAN_POINT('Ctrl Pts',(12.5,-0.140547257611399,4.45840101528927));
#14671=CARTESIAN_POINT('Ctrl Pts',(12.5,-0.156644205929787,4.44609879839914));
#14672=CARTESIAN_POINT('Ctrl Pts',(12.5,-0.17192740174072,4.43272977950413));
#14673=CARTESIAN_POINT('Ctrl Pts',(12.5,-0.186217277007305,4.41832740439832));
#14674=CARTESIAN_POINT('Origin',(15.1,0.,4.));
#14675=CARTESIAN_POINT('',(15.1,-1.16619037896906,2.5));
#14676=CARTESIAN_POINT('',(15.1,1.16619037896906,2.5));
#14677=CARTESIAN_POINT('',(15.1,1.25,2.5));
#14678=CARTESIAN_POINT('Origin',(15.1,0.,4.));
#14679=CARTESIAN_POINT('Origin',(15.1,0.,4.));
#14680=CARTESIAN_POINT('',(15.1,2.75545529808154E-17,5.725));
#14681=CARTESIAN_POINT('Origin',(15.1,0.,5.5));
#14682=CARTESIAN_POINT('',(15.1,1.5,4.225));
#14683=CARTESIAN_POINT('Origin',(15.1,1.5,4.));
#14684=CARTESIAN_POINT('',(15.1,-1.5,4.225));
#14685=CARTESIAN_POINT('Origin',(15.1,-1.5,4.));
#14686=CARTESIAN_POINT('Origin',(14.4,-1.5,4.));
#14687=CARTESIAN_POINT('',(14.5,-1.5,4.225));
#14688=CARTESIAN_POINT('Origin',(14.5,-1.5,4.));
#14689=CARTESIAN_POINT('',(14.4,-1.5,4.225));
#14690=CARTESIAN_POINT('Origin',(14.4,1.5,4.));
#14691=CARTESIAN_POINT('',(14.5,1.5,4.225));
#14692=CARTESIAN_POINT('Origin',(14.5,1.5,4.));
#14693=CARTESIAN_POINT('',(14.4,1.5,4.225));
#14694=CARTESIAN_POINT('Origin',(14.4,0.,5.5));
#14695=CARTESIAN_POINT('',(14.5,-2.75545529808154E-17,5.725));
#14696=CARTESIAN_POINT('Origin',(14.5,0.,5.5));
#14697=CARTESIAN_POINT('',(14.4,-2.75545529808154E-17,5.725));
#14698=CARTESIAN_POINT('Origin',(14.4,2.5,2.5));
#14699=CARTESIAN_POINT('',(14.5,1.16619037896906,2.5));
#14700=CARTESIAN_POINT('',(14.5,-1.16619037896906,2.5));
#14701=CARTESIAN_POINT('',(14.5,1.25,2.5));
#14702=CARTESIAN_POINT('',(14.5,1.16619037896906,2.5));
#14703=CARTESIAN_POINT('',(14.5,-1.16619037896906,2.5));
#14704=CARTESIAN_POINT('Origin',(14.5,0.,4.));
#14705=CARTESIAN_POINT('Origin',(14.5,0.,4.));
#14706=CARTESIAN_POINT('',(14.5,-1.34711147906209E-16,5.1));
#14707=CARTESIAN_POINT('Origin',(14.5,0.,4.));
#14708=CARTESIAN_POINT('Origin',(14.5,0.,4.));
#14709=CARTESIAN_POINT('Origin',(12.5,0.,4.));
#14710=CARTESIAN_POINT('Origin',(12.5,0.,4.));
#14711=CARTESIAN_POINT('',(12.5,-1.34711147906209E-16,5.1));
#14712=CARTESIAN_POINT('',(12.5,-1.34711147906209E-16,5.1));
#14713=CARTESIAN_POINT('Origin',(12.5,0.,4.));
#14714=CARTESIAN_POINT('Origin',(12.5,0.,4.));
#14715=CARTESIAN_POINT('',(0.,0.,0.));
#14716=CARTESIAN_POINT('Origin',(0.375,0.5,0.));
#14717=CARTESIAN_POINT('',(-0.375,0.5,-4.59242549680257E-17));
#14718=CARTESIAN_POINT('Origin',(0.,0.5,0.));
#14719=CARTESIAN_POINT('Origin',(0.,0.475,0.));
#14720=CARTESIAN_POINT('',(-0.425,0.45,-5.20474889637625E-17));
#14721=CARTESIAN_POINT('Origin',(0.,0.45,0.));
#14722=CARTESIAN_POINT('',(-0.4,0.475,-4.89858719658941E-17));
#14723=CARTESIAN_POINT('Origin',(0.,0.24,0.));
#14724=CARTESIAN_POINT('',(-0.425,0.0299999999999998,-5.20474889637625E-17));
#14725=CARTESIAN_POINT('Origin',(0.,0.0299999999999998,0.));
#14726=CARTESIAN_POINT('',(-0.425,0.24,-5.20474889637625E-17));
#14727=CARTESIAN_POINT('Origin',(0.,0.0150000000000001,0.));
#14728=CARTESIAN_POINT('',(-0.395,4.85722573273506E-17,-4.83735485663204E-17));
#14729=CARTESIAN_POINT('Origin',(0.,0.,0.));
#14730=CARTESIAN_POINT('',(-0.41,0.0150000000000001,-5.02105187650415E-17));
#14731=CARTESIAN_POINT('Origin',(0.27,0.,0.));
#14732=CARTESIAN_POINT('',(-0.27,0.,-3.30654635769785E-17));
#14733=CARTESIAN_POINT('Origin',(0.,0.,0.));
#14734=CARTESIAN_POINT('Origin',(0.,-0.02,0.));
#14735=CARTESIAN_POINT('',(-0.24505,-0.0498999999999999,3.00099698131059E-17));
#14736=CARTESIAN_POINT('Origin',(0.,-0.0498999999999999,0.));
#14737=CARTESIAN_POINT('',(-0.26,-0.02,-3.18408167778312E-17));
#14738=CARTESIAN_POINT('Origin',(0.,-0.995,0.));
#14739=CARTESIAN_POINT('',(-0.24505,-1.95495,3.00099698131059E-17));
#14740=CARTESIAN_POINT('Origin',(0.,-1.95495,0.));
#14741=CARTESIAN_POINT('',(-0.24505,-0.995,-3.00099698131059E-17));
#14742=CARTESIAN_POINT('Origin',(0.,-1.975,0.));
#14743=CARTESIAN_POINT('',(-0.2,-2.,-2.44929359829471E-17));
#14744=CARTESIAN_POINT('Origin',(0.,-2.,0.));
#14745=CARTESIAN_POINT('',(-0.225,-1.975,-2.75545529808154E-17));
#14746=CARTESIAN_POINT('Origin',(0.,-2.,0.));
#14747=CARTESIAN_POINT('Origin',(0.115470053837925,-0.5,-0.2));
#14748=CARTESIAN_POINT('',(0.23094010767585,-0.5,0.));
#14749=CARTESIAN_POINT('',(0.115470053837925,-0.5,-0.2));
#14750=CARTESIAN_POINT('',(0.23094010767585,-0.5,0.));
#14751=CARTESIAN_POINT('',(0.115470053837925,-0.8,-0.2));
#14752=CARTESIAN_POINT('',(0.115470053837925,-0.5,-0.2));
#14753=CARTESIAN_POINT('',(0.23094010767585,-0.8,0.));
#14754=CARTESIAN_POINT('',(0.23094010767585,-0.8,0.));
#14755=CARTESIAN_POINT('',(0.23094010767585,-0.5,0.));
#14756=CARTESIAN_POINT('Origin',(-0.115470053837925,-0.5,-0.2));
#14757=CARTESIAN_POINT('',(-0.115470053837925,-0.5,-0.2));
#14758=CARTESIAN_POINT('',(0.115470053837925,-0.5,-0.2));
#14759=CARTESIAN_POINT('',(-0.115470053837925,-0.8,-0.2));
#14760=CARTESIAN_POINT('',(-0.115470053837925,-0.5,-0.2));
#14761=CARTESIAN_POINT('',(0.115470053837925,-0.8,-0.2));
#14762=CARTESIAN_POINT('Origin',(-0.23094010767585,-0.5,-2.77555756156289E-17));
#14763=CARTESIAN_POINT('',(-0.23094010767585,-0.5,-2.82820063659975E-17));
#14764=CARTESIAN_POINT('',(-0.115470053837925,-0.5,-0.2));
#14765=CARTESIAN_POINT('',(-0.23094010767585,-0.8,-2.77555756156289E-17));
#14766=CARTESIAN_POINT('',(-0.23094010767585,-0.5,-2.82820063659975E-17));
#14767=CARTESIAN_POINT('',(-0.115470053837925,-0.8,-0.2));
#14768=CARTESIAN_POINT('Origin',(-0.115470053837925,-0.5,0.2));
#14769=CARTESIAN_POINT('',(-0.115470053837925,-0.5,0.2));
#14770=CARTESIAN_POINT('',(-0.23094010767585,-0.5,-2.82820063659975E-17));
#14771=CARTESIAN_POINT('',(-0.115470053837925,-0.8,0.2));
#14772=CARTESIAN_POINT('',(-0.115470053837925,-0.5,0.2));
#14773=CARTESIAN_POINT('',(-0.23094010767585,-0.8,-2.82820063659975E-17));
#14774=CARTESIAN_POINT('Origin',(0.115470053837925,-0.5,0.2));
#14775=CARTESIAN_POINT('',(0.115470053837925,-0.5,0.2));
#14776=CARTESIAN_POINT('',(-0.115470053837925,-0.5,0.2));
#14777=CARTESIAN_POINT('',(0.115470053837925,-0.8,0.2));
#14778=CARTESIAN_POINT('',(0.115470053837925,-0.5,0.2));
#14779=CARTESIAN_POINT('',(-0.115470053837925,-0.8,0.2));
#14780=CARTESIAN_POINT('Origin',(0.23094010767585,-0.5,0.));
#14781=CARTESIAN_POINT('',(0.115470053837925,-0.5,0.2));
#14782=CARTESIAN_POINT('',(0.115470053837925,-0.8,0.2));
#14783=CARTESIAN_POINT('Origin',(0.,-0.5,0.));
#14784=CARTESIAN_POINT('Origin',(0.,-0.8,0.));
#14785=CARTESIAN_POINT('',(0.,0.,0.));
#14786=CARTESIAN_POINT('Origin',(0.3,0.4,0.));
#14787=CARTESIAN_POINT('',(-0.3,0.4,-3.67394039744206E-17));
#14788=CARTESIAN_POINT('Origin',(0.,0.4,0.));
#14789=CARTESIAN_POINT('Origin',(0.,0.375,0.));
#14790=CARTESIAN_POINT('',(-0.35,0.35,-4.28626379701573E-17));
#14791=CARTESIAN_POINT('Origin',(0.,0.35,0.));
#14792=CARTESIAN_POINT('',(-0.325,0.375,-3.9801020972289E-17));
#14793=CARTESIAN_POINT('Origin',(0.,0.19,0.));
#14794=CARTESIAN_POINT('',(-0.35,0.03,-4.28626379701574E-17));
#14795=CARTESIAN_POINT('Origin',(0.,0.03,0.));
#14796=CARTESIAN_POINT('',(-0.35,0.19,-4.28626379701574E-17));
#14797=CARTESIAN_POINT('Origin',(0.,0.0149999999999999,0.));
#14798=CARTESIAN_POINT('',(-0.32,-3.29597460435593E-17,-3.91886975727153E-17));
#14799=CARTESIAN_POINT('Origin',(0.,0.,0.));
#14800=CARTESIAN_POINT('',(-0.335,0.0149999999999999,-4.10256677714363E-17));
#14801=CARTESIAN_POINT('Origin',(0.22,0.,0.));
#14802=CARTESIAN_POINT('',(-0.22,-6.93889390390723E-18,-2.69422295812418E-17));
#14803=CARTESIAN_POINT('Origin',(0.,0.,0.));
#14804=CARTESIAN_POINT('Origin',(0.,-0.02,0.));
#14805=CARTESIAN_POINT('',(-0.1954,-0.0492,2.39295984553393E-17));
#14806=CARTESIAN_POINT('Origin',(0.,-0.0492,0.));
#14807=CARTESIAN_POINT('',(-0.21,-0.02,-2.57175827820944E-17));
#14808=CARTESIAN_POINT('Origin',(0.,-0.8,0.));
#14809=CARTESIAN_POINT('',(-0.1954,-1.5646,2.39295984553393E-17));
#14810=CARTESIAN_POINT('Origin',(0.,-1.5646,0.));
#14811=CARTESIAN_POINT('',(-0.1954,-0.8,-2.39295984553393E-17));
#14812=CARTESIAN_POINT('Origin',(0.,-1.58,0.));
#14813=CARTESIAN_POINT('',(-0.16,-1.6,-1.95943487863577E-17));
#14814=CARTESIAN_POINT('Origin',(0.,-1.6,0.));
#14815=CARTESIAN_POINT('',(-0.18,-1.58,-2.20436423846524E-17));
#14816=CARTESIAN_POINT('Origin',(0.,-1.6,0.));
#14817=CARTESIAN_POINT('Origin',(0.0866025403784439,-0.4,-0.15));
#14818=CARTESIAN_POINT('',(0.173205080756888,-0.4,0.));
#14819=CARTESIAN_POINT('',(0.0866025403784439,-0.4,-0.15));
#14820=CARTESIAN_POINT('',(0.173205080756888,-0.4,0.));
#14821=CARTESIAN_POINT('',(0.0866025403784439,-0.64,-0.15));
#14822=CARTESIAN_POINT('',(0.0866025403784439,-0.4,-0.15));
#14823=CARTESIAN_POINT('',(0.173205080756888,-0.64,0.));
#14824=CARTESIAN_POINT('',(0.173205080756888,-0.64,0.));
#14825=CARTESIAN_POINT('',(0.173205080756888,-0.4,0.));
#14826=CARTESIAN_POINT('Origin',(-0.0866025403784438,-0.4,-0.15));
#14827=CARTESIAN_POINT('',(-0.0866025403784438,-0.4,-0.15));
#14828=CARTESIAN_POINT('',(0.0866025403784439,-0.4,-0.15));
#14829=CARTESIAN_POINT('',(-0.0866025403784438,-0.64,-0.15));
#14830=CARTESIAN_POINT('',(-0.0866025403784438,-0.4,-0.15));
#14831=CARTESIAN_POINT('',(0.0866025403784439,-0.64,-0.15));
#14832=CARTESIAN_POINT('Origin',(-0.173205080756888,-0.4,-2.77555756156289E-17));
#14833=CARTESIAN_POINT('',(-0.173205080756888,-0.4,-2.12115047744981E-17));
#14834=CARTESIAN_POINT('',(-0.0866025403784438,-0.4,-0.15));
#14835=CARTESIAN_POINT('',(-0.173205080756888,-0.64,-2.77555756156289E-17));
#14836=CARTESIAN_POINT('',(-0.173205080756888,-0.4,-2.12115047744981E-17));
#14837=CARTESIAN_POINT('',(-0.0866025403784438,-0.64,-0.15));
#14838=CARTESIAN_POINT('Origin',(-0.0866025403784439,-0.4,0.15));
#14839=CARTESIAN_POINT('',(-0.0866025403784439,-0.4,0.15));
#14840=CARTESIAN_POINT('',(-0.173205080756888,-0.4,-2.12115047744981E-17));
#14841=CARTESIAN_POINT('',(-0.0866025403784439,-0.64,0.15));
#14842=CARTESIAN_POINT('',(-0.0866025403784439,-0.4,0.15));
#14843=CARTESIAN_POINT('',(-0.173205080756888,-0.64,-2.12115047744981E-17));
#14844=CARTESIAN_POINT('Origin',(0.0866025403784439,-0.4,0.15));
#14845=CARTESIAN_POINT('',(0.0866025403784439,-0.4,0.15));
#14846=CARTESIAN_POINT('',(-0.0866025403784439,-0.4,0.15));
#14847=CARTESIAN_POINT('',(0.0866025403784439,-0.64,0.15));
#14848=CARTESIAN_POINT('',(0.0866025403784439,-0.4,0.15));
#14849=CARTESIAN_POINT('',(-0.0866025403784439,-0.64,0.15));
#14850=CARTESIAN_POINT('Origin',(0.173205080756888,-0.4,0.));
#14851=CARTESIAN_POINT('',(0.0866025403784439,-0.4,0.15));
#14852=CARTESIAN_POINT('',(0.0866025403784439,-0.64,0.15));
#14853=CARTESIAN_POINT('Origin',(0.,-0.4,-2.77555756156289E-17));
#14854=CARTESIAN_POINT('Origin',(0.,-0.64,-2.77555756156289E-17));
#14855=CARTESIAN_POINT('',(0.,0.,0.));
#14856=CARTESIAN_POINT('',(0.,0.,0.));
#14857=CARTESIAN_POINT('',(0.,0.,0.));
#14858=CARTESIAN_POINT('',(0.,0.,0.));
#14859=CARTESIAN_POINT('',(11.8,4.7,2.));
#14860=CARTESIAN_POINT('',(13.7,4.7,2.));
#14861=CARTESIAN_POINT('',(10.55,-3.,5.8));
#14862=CARTESIAN_POINT('',(10.55,3.,5.8));
#14863=CARTESIAN_POINT('',(15.1,-1.5,4.));
#14864=CARTESIAN_POINT('',(15.1,1.5,4.));
#14865=CARTESIAN_POINT('',(15.1,0.,5.5));
#14866=CARTESIAN_POINT('',(0.,0.,0.));
#14867=CARTESIAN_POINT('',(0.,0.,0.));
#14868=CARTESIAN_POINT('Origin',(4.,0.,4.));
#14869=CARTESIAN_POINT('',(4.12884541125756,8.40637486662632E-6,4.59405635738975));
#14870=CARTESIAN_POINT('',(4.02115458874249,-9.26662433349265E-6,4.59413599269206));
#14871=CARTESIAN_POINT('',(4.,-7.27562663373442E-17,4.5941));
#14872=CARTESIAN_POINT('',(4.,0.254721014554615,3.46322028700965));
#14873=CARTESIAN_POINT('Ctrl Pts',(4.12884541125756,8.40637486662632E-6,
4.59405635738975));
#14874=CARTESIAN_POINT('Ctrl Pts',(4.12564700130467,0.0398130654959074,
4.59407663624518));
#14875=CARTESIAN_POINT('Ctrl Pts',(4.12244859135178,0.079613792300143,4.59013569217808));
#14876=CARTESIAN_POINT('Ctrl Pts',(4.11925018139889,0.118599576779877,4.58219388355888));
#14877=CARTESIAN_POINT('Ctrl Pts',(4.11129754205509,0.215535206692688,4.56244709042845));
#14878=CARTESIAN_POINT('Ctrl Pts',(4.10334490271129,0.30743256945264,4.51796551073728));
#14879=CARTESIAN_POINT('Ctrl Pts',(4.09539226336748,0.383054411795556,4.45418672179759));
#14880=CARTESIAN_POINT('Ctrl Pts',(4.08743962402367,0.458676254138472,4.3904079328579));
#14881=CARTESIAN_POINT('Ctrl Pts',(4.07948698467986,0.518022576064352,4.30733193466969));
#14882=CARTESIAN_POINT('Ctrl Pts',(4.07153434533606,0.553840407547632,4.21511760274296));
#14883=CARTESIAN_POINT('Ctrl Pts',(4.06358170599225,0.589658239030912,4.12290327081622));
#14884=CARTESIAN_POINT('Ctrl Pts',(4.05562906664845,0.601947580071592,4.02155060515096));
#14885=CARTESIAN_POINT('Ctrl Pts',(4.04767642730464,0.589200356533535,3.92344812692479));
#14886=CARTESIAN_POINT('Ctrl Pts',(4.03972378796084,0.576453132995478,3.82534564869861));
#14887=CARTESIAN_POINT('Ctrl Pts',(4.03177114861703,0.538669344878685,3.73049335791153));
#14888=CARTESIAN_POINT('Ctrl Pts',(4.02381850927322,0.480479105222089,3.65049437695417));
#14889=CARTESIAN_POINT('Ctrl Pts',(4.01587900618215,0.422384984811151,3.57062753914914));
#14890=CARTESIAN_POINT('Ctrl Pts',(4.00793950309107,0.343951772361455,3.50556498199611));
#14891=CARTESIAN_POINT('Ctrl Pts',(4.,0.254721014554615,3.46322028700965));
#14892=CARTESIAN_POINT('',(4.,0.254694598474614,4.53673594206822));
#14893=CARTESIAN_POINT('Origin',(4.,0.,4.));
#14894=CARTESIAN_POINT('Ctrl Pts',(3.99999999999998,0.254694598474614,4.53673594206822));
#14895=CARTESIAN_POINT('Ctrl Pts',(4.00705152958082,0.175425736340139,4.5743509952638));
#14896=CARTESIAN_POINT('Ctrl Pts',(4.01410305916165,0.0876996967667308,
4.59405101338575));
#14897=CARTESIAN_POINT('Ctrl Pts',(4.02115458874249,-9.26662433349265E-6,
4.59413599269206));
#14898=CARTESIAN_POINT('Origin',(4.,0.,4.));
#14899=CARTESIAN_POINT('',(4.42884541125756,-2.46302091461148E-6,4.59415045696459));
#14900=CARTESIAN_POINT('',(4.32115458874249,3.58587963140688E-6,4.59404994535016));
#14901=CARTESIAN_POINT('',(4.,-7.27562663373442E-17,4.5941));
#14902=CARTESIAN_POINT('Ctrl Pts',(4.42884541125756,-2.46302091461148E-6,
4.59415045696459));
#14903=CARTESIAN_POINT('Ctrl Pts',(4.42107867343035,0.0966117732708647,
4.59412799973471));
#14904=CARTESIAN_POINT('Ctrl Pts',(4.41331193560314,0.193236775309615,4.57009608476161));
#14905=CARTESIAN_POINT('Ctrl Pts',(4.40554519777592,0.278573173318151,4.52479781884576));
#14906=CARTESIAN_POINT('Ctrl Pts',(4.39759255843212,0.36595214906825,4.47841531183407));
#14907=CARTESIAN_POINT('Ctrl Pts',(4.38963991908831,0.441495654419193,4.40973622444741));
#14908=CARTESIAN_POINT('Ctrl Pts',(4.3816872797445,0.495967466205845,4.32715751007026));
#14909=CARTESIAN_POINT('Ctrl Pts',(4.3737346404007,0.550439277992498,4.24457879569311));
#14910=CARTESIAN_POINT('Ctrl Pts',(4.36578200105689,0.58383939621486,4.14810045432546));
#14911=CARTESIAN_POINT('Ctrl Pts',(4.35782936171309,0.59208420294366,4.04951827803692));
#14912=CARTESIAN_POINT('Ctrl Pts',(4.34987672236928,0.600329009672459,3.95093610174838));
#14913=CARTESIAN_POINT('Ctrl Pts',(4.34192408302547,0.583418504907695,3.85025009053894));
#14914=CARTESIAN_POINT('Ctrl Pts',(4.33397144368167,0.54342022548472,3.75977047903001));
#14915=CARTESIAN_POINT('Ctrl Pts',(4.32601880433786,0.503421946061746,3.66929086752108));
#14916=CARTESIAN_POINT('Ctrl Pts',(4.31806616499406,0.440335891980562,3.58901765571266));
#14917=CARTESIAN_POINT('Ctrl Pts',(4.31011352565025,0.361875197644003,3.52876534000234));
#14918=CARTESIAN_POINT('Ctrl Pts',(4.30216088630644,0.283414503307443,3.46851302429202));
#14919=CARTESIAN_POINT('Ctrl Pts',(4.29420824696263,0.189579168715509,3.4282816046798));
#14920=CARTESIAN_POINT('Ctrl Pts',(4.28625560761883,0.0918418319479975,
3.41298991457491));
#14921=CARTESIAN_POINT('Ctrl Pts',(4.27830296827502,-0.00589550481951406,
3.39769822447003));
#14922=CARTESIAN_POINT('Ctrl Pts',(4.27035032893122,-0.107534843762603,
3.4073462638725));
#14923=CARTESIAN_POINT('Ctrl Pts',(4.26239768958741,-0.200649373295791,
3.44075443909651));
#14924=CARTESIAN_POINT('Ctrl Pts',(4.25444505024361,-0.293763902828979,
3.47416261432052));
#14925=CARTESIAN_POINT('Ctrl Pts',(4.24649241089979,-0.378353622952266,
3.53133092536608));
#14926=CARTESIAN_POINT('Ctrl Pts',(4.23853977155599,-0.444076322467606,
3.60526974769923));
#14927=CARTESIAN_POINT('Ctrl Pts',(4.23058713221218,-0.509799021982947,
3.67920857003239));
#14928=CARTESIAN_POINT('Ctrl Pts',(4.22263449286838,-0.556654700890342,
3.76991790365313));
#14929=CARTESIAN_POINT('Ctrl Pts',(4.21468185352458,-0.578914549750806,
3.86630733464992));
#14930=CARTESIAN_POINT('Ctrl Pts',(4.20672921418077,-0.601174398611269,
3.96269676564671));
#14931=CARTESIAN_POINT('Ctrl Pts',(4.19877657483696,-0.598838417424802,
4.06476629401955));
#14932=CARTESIAN_POINT('Ctrl Pts',(4.19082393549315,-0.5721923335546,4.16003645884502));
#14933=CARTESIAN_POINT('Ctrl Pts',(4.18287129614934,-0.545546249684398,
4.25530662367048));
#14934=CARTESIAN_POINT('Ctrl Pts',(4.17491865680554,-0.494590063130461,
4.34377742494856));
#14935=CARTESIAN_POINT('Ctrl Pts',(4.16696601746173,-0.425553631634784,
4.41463223618795));
#14936=CARTESIAN_POINT('Ctrl Pts',(4.15901337811793,-0.356517200139107,
4.48548704742733));
#14937=CARTESIAN_POINT('Ctrl Pts',(4.15106073877413,-0.269400523701689,
4.53872586862801));
#14938=CARTESIAN_POINT('Ctrl Pts',(4.14310809943032,-0.174855236950146,
4.56783927594351));
#14939=CARTESIAN_POINT('Ctrl Pts',(4.1383538700394,-0.118334381217266,4.5852437891806));
#14940=CARTESIAN_POINT('Ctrl Pts',(4.13359964064848,-0.0591586432141876,
4.59402621418361));
#14941=CARTESIAN_POINT('Ctrl Pts',(4.12884541125756,8.40637486662632E-6,
4.59405635738975));
#14942=CARTESIAN_POINT('Ctrl Pts',(4.02115458874249,-9.26662433349265E-6,
4.59413599269206));
#14943=CARTESIAN_POINT('Ctrl Pts',(4.02205569850546,-0.0112175303500608,
4.59414685213492));
#14944=CARTESIAN_POINT('Ctrl Pts',(4.02295680826843,-0.0224255152200988,
4.5938373961197));
#14945=CARTESIAN_POINT('Ctrl Pts',(4.0238579180314,-0.0336155370699344,
4.59320407706013));
#14946=CARTESIAN_POINT('Ctrl Pts',(4.03181055737521,-0.132371772633995,
4.58761479340425));
#14947=CARTESIAN_POINT('Ctrl Pts',(4.03976319671902,-0.229728915328813,
4.55680066053817));
#14948=CARTESIAN_POINT('Ctrl Pts',(4.04771583606282,-0.31374319278985,4.50455967689729));
#14949=CARTESIAN_POINT('Ctrl Pts',(4.05566847540663,-0.397757470250888,
4.4523186932564));
#14950=CARTESIAN_POINT('Ctrl Pts',(4.06362111475043,-0.468428882478145,
4.37865085884071));
#14951=CARTESIAN_POINT('Ctrl Pts',(4.07157375409424,-0.517135915630147,
4.29254879227412));
#14952=CARTESIAN_POINT('Ctrl Pts',(4.07952639343804,-0.565842948782149,
4.20644672570752));
#14953=CARTESIAN_POINT('Ctrl Pts',(4.08747903278185,-0.592585602858896,
4.10791042699003));
#14954=CARTESIAN_POINT('Ctrl Pts',(4.09543167212566,-0.594084460855775,
4.00899459728238));
#14955=CARTESIAN_POINT('Ctrl Pts',(4.10338431146947,-0.595583318852653,
3.91007876757474));
#14956=CARTESIAN_POINT('Ctrl Pts',(4.11133695081327,-0.571838380769662,
3.81078340687695));
#14957=CARTESIAN_POINT('Ctrl Pts',(4.11928959015708,-0.525757920758293,
3.72324489380985));
#14958=CARTESIAN_POINT('Ctrl Pts',(4.12724222950088,-0.479677460746923,
3.63570638074275));
#14959=CARTESIAN_POINT('Ctrl Pts',(4.13519486884469,-0.411261478807175,
3.55992471530633));
#14960=CARTESIAN_POINT('Ctrl Pts',(4.1431475081885,-0.328872047298013,3.50516726345229));
#14961=CARTESIAN_POINT('Ctrl Pts',(4.1511001475323,-0.246482615788851,3.45040981159825));
#14962=CARTESIAN_POINT('Ctrl Pts',(4.15905278687611,-0.150119734710276,
3.41667657332659));
#14963=CARTESIAN_POINT('Ctrl Pts',(4.16700542621992,-0.0515665150750243,
3.40809082437526));
#14964=CARTESIAN_POINT('Ctrl Pts',(4.17495806556372,0.0469867045602276,
3.39950507542393));
#14965=CARTESIAN_POINT('Ctrl Pts',(4.18291070490753,0.147730262752155,3.41606681579293));
#14966=CARTESIAN_POINT('Ctrl Pts',(4.19086334425134,0.238347648045887,3.45575171487277));
#14967=CARTESIAN_POINT('Ctrl Pts',(4.19881598359514,0.32896503333962,3.49543661395261));
#14968=CARTESIAN_POINT('Ctrl Pts',(4.20676862293895,0.409456245735157,3.55824467174328));
#14969=CARTESIAN_POINT('Ctrl Pts',(4.21472126228276,0.469979735422806,3.63649644709345));
#14970=CARTESIAN_POINT('Ctrl Pts',(4.22267390162656,0.530503225110456,3.71474822244363));
#14971=CARTESIAN_POINT('Ctrl Pts',(4.23062654097037,0.571058992090217,3.80844371535332));
#14972=CARTESIAN_POINT('Ctrl Pts',(4.23857918031417,0.586688754827568,3.90612753493601));
#14973=CARTESIAN_POINT('Ctrl Pts',(4.24653181965798,0.602318517564919,4.0038113545187));
#14974=CARTESIAN_POINT('Ctrl Pts',(4.25448445900178,0.593022276059861,4.10548350077438));
#14975=CARTESIAN_POINT('Ctrl Pts',(4.26243709834559,0.559936509464549,4.19871308474845));
#14976=CARTESIAN_POINT('Ctrl Pts',(4.2703897376894,0.526850742869238,4.29194266872251));
#14977=CARTESIAN_POINT('Ctrl Pts',(4.27834237703321,0.469975451183674,4.37672969041494));
#14978=CARTESIAN_POINT('Ctrl Pts',(4.28629501637701,0.396264473279151,4.44270782630825));
#14979=CARTESIAN_POINT('Ctrl Pts',(4.29424765572082,0.322553495374627,4.50868596220156));
#14980=CARTESIAN_POINT('Ctrl Pts',(4.30220029506462,0.232006831251144,4.55585521229574));
#14981=CARTESIAN_POINT('Ctrl Pts',(4.31015293440843,0.135695012128791,4.57844846968215));
#14982=CARTESIAN_POINT('Ctrl Pts',(4.31382015251978,0.0912825306677821,
4.58886694826517));
#14983=CARTESIAN_POINT('Ctrl Pts',(4.31748737063114,0.0456441298716245,
4.59405951624442));
#14984=CARTESIAN_POINT('Ctrl Pts',(4.32115458874249,3.58587963140688E-6,
4.59404994535016));
#14985=CARTESIAN_POINT('Origin',(4.,0.,4.));
#14986=CARTESIAN_POINT('',(4.72884541125756,-4.67700812217808E-6,4.59405084457266));
#14987=CARTESIAN_POINT('',(4.62115458874249,3.7232086238465E-6,4.59414939806979));
#14988=CARTESIAN_POINT('',(4.,-7.27562663373442E-17,4.5941));
#14989=CARTESIAN_POINT('Ctrl Pts',(4.72884541125756,-4.67700812217808E-6,
4.59405084457266));
#14990=CARTESIAN_POINT('Ctrl Pts',(4.72446298489983,0.0545367878429411,
4.59403588702548));
#14991=CARTESIAN_POINT('Ctrl Pts',(4.7200805585421,0.10908225468116,4.58659074407712));
#14992=CARTESIAN_POINT('Ctrl Pts',(4.71569813218437,0.16154350694756,4.57176871113812));
#14993=CARTESIAN_POINT('Ctrl Pts',(4.70774549284056,0.256743148594298,4.54487167450041));
#14994=CARTESIAN_POINT('Ctrl Pts',(4.69979285349676,0.345079446524661,4.4936824501733));
#14995=CARTESIAN_POINT('Ctrl Pts',(4.69184021415295,0.415752085200636,4.42445961801412));
#14996=CARTESIAN_POINT('Ctrl Pts',(4.68388757480915,0.486424723876611,4.35523678585494));
#14997=CARTESIAN_POINT('Ctrl Pts',(4.67593493546534,0.539433703298198,4.26798034586369));
#14998=CARTESIAN_POINT('Ctrl Pts',(4.66798229612153,0.568297953762936,4.17335858623793));
#14999=CARTESIAN_POINT('Ctrl Pts',(4.66002965677773,0.597162204227674,4.07873682661218));
#15000=CARTESIAN_POINT('Ctrl Pts',(4.65207701743392,0.601881725735563,3.97674974735193));
#15001=CARTESIAN_POINT('Ctrl Pts',(4.64412437809011,0.581879492504365,3.87986665793328));
#15002=CARTESIAN_POINT('Ctrl Pts',(4.63617173874631,0.561877259273167,3.78298356851463));
#15003=CARTESIAN_POINT('Ctrl Pts',(4.6282190994025,0.517153271302883,3.69120446893757));
#15004=CARTESIAN_POINT('Ctrl Pts',(4.6202664600587,0.453175645250056,3.61575060413089));
#15005=CARTESIAN_POINT('Ctrl Pts',(4.61231382071489,0.389198019197228,3.5402967393242));
#15006=CARTESIAN_POINT('Ctrl Pts',(4.60436118137108,0.305966755061857,3.48116810928789));
#15007=CARTESIAN_POINT('Ctrl Pts',(4.59640854202727,0.213658008474022,3.4455939943611));
#15008=CARTESIAN_POINT('Ctrl Pts',(4.58845590268347,0.121349261886187,3.41001987943431));
#15009=CARTESIAN_POINT('Ctrl Pts',(4.58050326333966,0.0199630328458878,
3.39800027961704));
#15010=CARTESIAN_POINT('Ctrl Pts',(4.57255062399586,-0.0781048312986516,
3.41100475468789));
#15011=CARTESIAN_POINT('Ctrl Pts',(4.56459798465205,-0.17617269544319,3.42400922975875));
#15012=CARTESIAN_POINT('Ctrl Pts',(4.55664534530825,-0.270922194691968,
3.46203777971774));
#15013=CARTESIAN_POINT('Ctrl Pts',(4.54869270596444,-0.350768912290741,
3.52044089639904));
#15014=CARTESIAN_POINT('Ctrl Pts',(4.54074006662063,-0.430615629889515,
3.57884401308035));
#15015=CARTESIAN_POINT('Ctrl Pts',(4.53278742727683,-0.495559565838284,
3.65762169648397));
#15016=CARTESIAN_POINT('Ctrl Pts',(4.52483478793302,-0.537660439465301,
3.74714230187364));
#15017=CARTESIAN_POINT('Ctrl Pts',(4.51688214858921,-0.579761313092318,
3.8366629072633));
#15018=CARTESIAN_POINT('Ctrl Pts',(4.50892950924541,-0.599019124397585,
3.936926434639));
#15019=CARTESIAN_POINT('Ctrl Pts',(4.5009768699016,-0.593079343631488,4.03567430223551));
#15020=CARTESIAN_POINT('Ctrl Pts',(4.49302423055779,-0.587139562865391,
4.13442216983203));
#15021=CARTESIAN_POINT('Ctrl Pts',(4.48507159121399,-0.556002190027932,
4.23165437764937));
#15022=CARTESIAN_POINT('Ctrl Pts',(4.47711895187018,-0.503474193090318,
4.31548296397124));
#15023=CARTESIAN_POINT('Ctrl Pts',(4.46916631252638,-0.450946196152703,
4.39931155029312));
#15024=CARTESIAN_POINT('Ctrl Pts',(4.46121367318257,-0.377027575114933,
4.46973651511953));
#15025=CARTESIAN_POINT('Ctrl Pts',(4.45326103383876,-0.290755888038263,
4.51814744739689));
#15026=CARTESIAN_POINT('Ctrl Pts',(4.44530839449495,-0.204484200961595,
4.56655837967425));
#15027=CARTESIAN_POINT('Ctrl Pts',(4.43735575515115,-0.105859447846027,
4.59295527940255));
#15028=CARTESIAN_POINT('Ctrl Pts',(4.42940311580734,-0.00693984821361558,
4.59411076594835));
#15029=CARTESIAN_POINT('Ctrl Pts',(4.42921721429075,-0.0046274959494805,
4.59413777669183));
#15030=CARTESIAN_POINT('Ctrl Pts',(4.42903131277416,-0.00231498256911503,
4.59415099449182));
#15031=CARTESIAN_POINT('Ctrl Pts',(4.42884541125756,-2.46302091461148E-6,
4.59415045696459));
#15032=CARTESIAN_POINT('Ctrl Pts',(4.32115458874249,3.58587963140688E-6,
4.59404994535016));
#15033=CARTESIAN_POINT('Ctrl Pts',(4.32544000997495,-0.0533308355660028,
4.59403876103764));
#15034=CARTESIAN_POINT('Ctrl Pts',(4.3297254312074,-0.106668183692779,4.58692369872924));
#15035=CARTESIAN_POINT('Ctrl Pts',(4.33401085243985,-0.158055593105036,
4.57274269264177));
#15036=CARTESIAN_POINT('Ctrl Pts',(4.34196349178366,-0.253417405095285,
4.54642639353635));
#15037=CARTESIAN_POINT('Ctrl Pts',(4.34991613112746,-0.342064054954561,
4.49577653064689));
#15038=CARTESIAN_POINT('Ctrl Pts',(4.35786877047127,-0.413157291282808,
4.42698573291487));
#15039=CARTESIAN_POINT('Ctrl Pts',(4.36582140981507,-0.484250527611055,
4.35819493518285));
#15040=CARTESIAN_POINT('Ctrl Pts',(4.37377404915888,-0.537790350408272,
4.27126320260829));
#15041=CARTESIAN_POINT('Ctrl Pts',(4.38172668850269,-0.567230782432438,
4.17681912699824));
#15042=CARTESIAN_POINT('Ctrl Pts',(4.3896793278465,-0.596671214456604,4.0823750513882));
#15043=CARTESIAN_POINT('Ctrl Pts',(4.3976319671903,-0.602012255707717,3.98041863274268));
#15044=CARTESIAN_POINT('Ctrl Pts',(4.40558460653411,-0.582600893642323,
3.88341542999892));
#15045=CARTESIAN_POINT('Ctrl Pts',(4.41353724587791,-0.563189531576929,
3.78641222725516));
#15046=CARTESIAN_POINT('Ctrl Pts',(4.42148988522172,-0.519025766195027,
3.69436224041317));
#15047=CARTESIAN_POINT('Ctrl Pts',(4.42944252456553,-0.455509217992651,
3.61851983504546));
#15048=CARTESIAN_POINT('Ctrl Pts',(4.43739516390933,-0.391992669790276,
3.54267742967776));
#15049=CARTESIAN_POINT('Ctrl Pts',(4.44534780325314,-0.309123338767427,
3.48304260578434));
#15050=CARTESIAN_POINT('Ctrl Pts',(4.45330044259694,-0.217033129998519,
3.44690653227429));
#15051=CARTESIAN_POINT('Ctrl Pts',(4.46125308194075,-0.12494292122961,3.41077045876423));
#15052=CARTESIAN_POINT('Ctrl Pts',(4.46920572128456,-0.0236318347146405,
3.39813313563753));
#15053=CARTESIAN_POINT('Ctrl Pts',(4.47715836062837,0.074513469760962,3.41053964803971));
#15054=CARTESIAN_POINT('Ctrl Pts',(4.48511099997217,0.172658774236564,3.42294616044189));
#15055=CARTESIAN_POINT('Ctrl Pts',(4.49306363931598,0.2676382966728,3.46039650837296));
#15056=CARTESIAN_POINT('Ctrl Pts',(4.50101627865978,0.34783949666059,3.51831187658845));
#15057=CARTESIAN_POINT('Ctrl Pts',(4.50896891800359,0.428040696648381,3.57622724480394));
#15058=CARTESIAN_POINT('Ctrl Pts',(4.51692155734739,0.493463574187728,3.65460763330386));
#15059=CARTESIAN_POINT('Ctrl Pts',(4.5248741966912,0.536109291561612,3.74386997215216));
#15060=CARTESIAN_POINT('Ctrl Pts',(4.53282683603501,0.578755008935497,3.83313231100046));
#15061=CARTESIAN_POINT('Ctrl Pts',(4.54077947537881,0.598623566143919,3.93327660019715));
#15062=CARTESIAN_POINT('Ctrl Pts',(4.54873211472262,0.593285761408823,4.03205883640902));
#15063=CARTESIAN_POINT('Ctrl Pts',(4.55668475406643,0.587947956673727,4.1308410726209));
#15064=CARTESIAN_POINT('Ctrl Pts',(4.56463739341024,0.557403789995114,4.22826125584796));
#15065=CARTESIAN_POINT('Ctrl Pts',(4.57259003275404,0.505387701781775,4.31240844187621));
#15066=CARTESIAN_POINT('Ctrl Pts',(4.58054267209785,0.453371613568435,4.39655562790445));
#15067=CARTESIAN_POINT('Ctrl Pts',(4.58849531144165,0.37988360382037,4.46742981673387));
#15068=CARTESIAN_POINT('Ctrl Pts',(4.59644795078546,0.293908582600447,4.51636567348148));
#15069=CARTESIAN_POINT('Ctrl Pts',(4.60440059012926,0.207933561380525,4.56530153022909));
#15070=CARTESIAN_POINT('Ctrl Pts',(4.61235322947307,0.109471528688745,4.59229905489488));
#15071=CARTESIAN_POINT('Ctrl Pts',(4.62030586881688,0.01056080905581,4.59405743239568));
#15072=CARTESIAN_POINT('Ctrl Pts',(4.62058877545875,0.00704216595801619,
4.59411998479525));
#15073=CARTESIAN_POINT('Ctrl Pts',(4.62087168210062,0.00352295504485493,
4.59415059693914));
#15074=CARTESIAN_POINT('Ctrl Pts',(4.62115458874249,3.7232086238465E-6,
4.59414939806979));
#15075=CARTESIAN_POINT('Origin',(4.,0.,4.));
#15076=CARTESIAN_POINT('',(5.02884541125756,1.1583539301252E-5,4.59413174414479));
#15077=CARTESIAN_POINT('',(4.92115458874249,-9.52916733652962E-6,4.59405847898621));
#15078=CARTESIAN_POINT('',(4.,-7.27562663373442E-17,4.5941));
#15079=CARTESIAN_POINT('Ctrl Pts',(5.02884541125756,1.1583539301252E-5,
4.59413174414479));
#15080=CARTESIAN_POINT('Ctrl Pts',(5.02784729636931,0.0124287555737821,
4.59414271605904));
#15081=CARTESIAN_POINT('Ctrl Pts',(5.02684918148107,0.024845254523583,4.59376142828251));
#15082=CARTESIAN_POINT('Ctrl Pts',(5.02585106659282,0.0372368329321061,
4.59298328977014));
#15083=CARTESIAN_POINT('Ctrl Pts',(5.01789842724901,0.135968707532707,4.58678334723719));
#15084=CARTESIAN_POINT('Ctrl Pts',(5.00994578790521,0.233118536601742,4.55538989360237));
#15085=CARTESIAN_POINT('Ctrl Pts',(5.0019931485614,0.316808430381418,4.50264120614281));
#15086=CARTESIAN_POINT('Ctrl Pts',(4.9940405092176,0.400498324161095,4.44989251868324));
#15087=CARTESIAN_POINT('Ctrl Pts',(4.98608786987379,0.470728282651411,4.37578859739892));
#15088=CARTESIAN_POINT('Ctrl Pts',(4.97813523052998,0.518911736914097,4.289389655942));
#15089=CARTESIAN_POINT('Ctrl Pts',(4.97018259118617,0.567095191176782,4.20299071448508));
#15090=CARTESIAN_POINT('Ctrl Pts',(4.96222995184237,0.593232141211837,4.10429675285556));
#15091=CARTESIAN_POINT('Ctrl Pts',(4.95427731249856,0.594126988899363,4.00537445204741));
#15092=CARTESIAN_POINT('Ctrl Pts',(4.94632467315476,0.595021836586889,3.90645215123927));
#15093=CARTESIAN_POINT('Ctrl Pts',(4.93837203381095,0.570674581926886,3.80730151125251));
#15094=CARTESIAN_POINT('Ctrl Pts',(4.93041939446714,0.524062008404491,3.72004504823011));
#15095=CARTESIAN_POINT('Ctrl Pts',(4.92246675512334,0.477449434882097,3.6327885852077));
#15096=CARTESIAN_POINT('Ctrl Pts',(4.91451411577953,0.408571542497308,3.55742629914966));
#15097=CARTESIAN_POINT('Ctrl Pts',(4.90656147643572,0.325849591692228,3.50317225594031));
#15098=CARTESIAN_POINT('Ctrl Pts',(4.89860883709192,0.243127640887147,3.44891821273095));
#15099=CARTESIAN_POINT('Ctrl Pts',(4.89065619774811,0.146561631661773,3.41577241237029));
#15100=CARTESIAN_POINT('Ctrl Pts',(4.88270355840431,0.0479580738465473,
3.40778738038914));
#15101=CARTESIAN_POINT('Ctrl Pts',(4.8747509190605,-0.0506454839686783,
3.39980234840799));
#15102=CARTESIAN_POINT('Ctrl Pts',(4.86679827971669,-0.151286590373755,
3.41697808480634));
#15103=CARTESIAN_POINT('Ctrl Pts',(4.85884564037289,-0.241660499406316,
3.45721462188069));
#15104=CARTESIAN_POINT('Ctrl Pts',(4.85089300102908,-0.332034408438876,
3.49745115895503));
#15105=CARTESIAN_POINT('Ctrl Pts',(4.84294036168527,-0.41214112009892,3.56074849670536));
#15106=CARTESIAN_POINT('Ctrl Pts',(4.83498772234147,-0.472186497854497,
3.63936767349926));
#15107=CARTESIAN_POINT('Ctrl Pts',(4.82703508299766,-0.532231875610076,
3.71798685029316));
#15108=CARTESIAN_POINT('Ctrl Pts',(4.81908244365386,-0.572215919461187,
3.81192786613063));
#15109=CARTESIAN_POINT('Ctrl Pts',(4.81112980431005,-0.587250035475296,
3.9097051523746));
#15110=CARTESIAN_POINT('Ctrl Pts',(4.80317716496624,-0.602284151489406,
4.00748243861856));
#15111=CARTESIAN_POINT('Ctrl Pts',(4.79522452562244,-0.592368339666514,
4.10909599526903));
#15112=CARTESIAN_POINT('Ctrl Pts',(4.78727188627863,-0.558714943052599,
4.20212218107662));
#15113=CARTESIAN_POINT('Ctrl Pts',(4.77931924693482,-0.525061546438685,
4.2951483668842));
#15114=CARTESIAN_POINT('Ctrl Pts',(4.77136660759101,-0.467670565033749,
4.37958718184891));
#15115=CARTESIAN_POINT('Ctrl Pts',(4.76341396824721,-0.393558827964045,
4.44511483080773));
#15116=CARTESIAN_POINT('Ctrl Pts',(4.7554613289034,-0.319447090894342,4.51064247976655));
#15117=CARTESIAN_POINT('Ctrl Pts',(4.7475086895596,-0.228614598159871,4.55725896271948));
#15118=CARTESIAN_POINT('Ctrl Pts',(4.73955605021579,-0.13216685911108,4.5792647797218));
#15119=CARTESIAN_POINT('Ctrl Pts',(4.73598583722972,-0.0888681559330128,
4.58914394690572));
#15120=CARTESIAN_POINT('Ctrl Pts',(4.73241562424364,-0.0444377444908,4.59406302997518));
#15121=CARTESIAN_POINT('Ctrl Pts',(4.72884541125756,-4.67700812217808E-6,
4.59405084457266));
#15122=CARTESIAN_POINT('Ctrl Pts',(4.62115458874249,3.7232086238465E-6,
4.59414939806979));
#15123=CARTESIAN_POINT('Ctrl Pts',(4.62882432144443,-0.0954043143036648,
4.59411689615543));
#15124=CARTESIAN_POINT('Ctrl Pts',(4.63649405414636,-0.190827729806029,
4.57070400848325));
#15125=CARTESIAN_POINT('Ctrl Pts',(4.6441637868483,-0.275369369969159,4.52648596729292));
#15126=CARTESIAN_POINT('Ctrl Pts',(4.65211642619211,-0.363029422787103,
4.48063689435358));
#15127=CARTESIAN_POINT('Ctrl Pts',(4.66006906553591,-0.438990121848901,
4.4124195181391));
#15128=CARTESIAN_POINT('Ctrl Pts',(4.66802170487971,-0.493964237128006,
4.33017434199545));
#15129=CARTESIAN_POINT('Ctrl Pts',(4.67597434422352,-0.548938352407109,
4.24792916585179));
#15130=CARTESIAN_POINT('Ctrl Pts',(4.68392698356733,-0.582925883903521,
4.15165618977896));
#15131=CARTESIAN_POINT('Ctrl Pts',(4.69187962291114,-0.591771392992132,
4.05312609631255));
#15132=CARTESIAN_POINT('Ctrl Pts',(4.69983226225494,-0.600616902080743,
3.95459600284613));
#15133=CARTESIAN_POINT('Ctrl Pts',(4.70778490159875,-0.584320388761555,
3.85380879198612));
#15134=CARTESIAN_POINT('Ctrl Pts',(4.71573754094256,-0.544874323741249,
3.76308707295491));
#15135=CARTESIAN_POINT('Ctrl Pts',(4.72369018028636,-0.505428258720944,
3.6723653539237));
#15136=CARTESIAN_POINT('Ctrl Pts',(4.73164281963017,-0.442832641999522,
3.59170912672127));
#15137=CARTESIAN_POINT('Ctrl Pts',(4.73959545897397,-0.364740640256699,
3.53097971363863));
#15138=CARTESIAN_POINT('Ctrl Pts',(4.74754809831778,-0.286648638513876,
3.47025030055599));
#15139=CARTESIAN_POINT('Ctrl Pts',(4.75550073766158,-0.193060251749651,
3.42944770159313));
#15140=CARTESIAN_POINT('Ctrl Pts',(4.76345337700539,-0.095417934894009,
3.41356059019365));
#15141=CARTESIAN_POINT('Ctrl Pts',(4.7714060163492,0.00222438196163176,
3.39767347879416));
#15142=CARTESIAN_POINT('Ctrl Pts',(4.77935865569301,0.10392062890869,3.40670185495805));
#15143=CARTESIAN_POINT('Ctrl Pts',(4.78731129503681,0.19723705468272,3.43954187673519));
#15144=CARTESIAN_POINT('Ctrl Pts',(4.79526393438062,0.290553480456751,3.47238189851233));
#15145=CARTESIAN_POINT('Ctrl Pts',(4.80321657372443,0.375490085057754,3.52903356590271));
#15146=CARTESIAN_POINT('Ctrl Pts',(4.81116921306823,0.441662211759978,3.60257044098769));
#15147=CARTESIAN_POINT('Ctrl Pts',(4.81912185241204,0.507834338462201,3.67610731607267));
#15148=CARTESIAN_POINT('Ctrl Pts',(4.82707449175584,0.555241987265645,3.76652939885225));
#15149=CARTESIAN_POINT('Ctrl Pts',(4.83502713109965,0.57808892742485,3.86278135818256));
#15150=CARTESIAN_POINT('Ctrl Pts',(4.84297977044346,0.600935867584054,3.95903331751286));
#15151=CARTESIAN_POINT('Ctrl Pts',(4.85093240978726,0.599222099099018,4.0611151533939));
#15152=CARTESIAN_POINT('Ctrl Pts',(4.85888504913107,0.573157153508111,4.15654597106253));
#15153=CARTESIAN_POINT('Ctrl Pts',(4.86683768847488,0.547092207917203,4.25197678873116));
#15154=CARTESIAN_POINT('Ctrl Pts',(4.87479032781868,0.496676085220424,4.34075658818739));
#15155=CARTESIAN_POINT('Ctrl Pts',(4.88274296716249,0.428072843071251,4.41203082979109));
#15156=CARTESIAN_POINT('Ctrl Pts',(4.89069560650629,0.359469600922078,4.48330507139479));
#15157=CARTESIAN_POINT('Ctrl Pts',(4.8986482458501,0.272679239320511,4.53707375514596));
#15158=CARTESIAN_POINT('Ctrl Pts',(4.90660088519391,0.178313062033339,4.56676292714126));
#15159=CARTESIAN_POINT('Ctrl Pts',(4.9114521197101,0.120748216373203,4.58487378690922));
#15160=CARTESIAN_POINT('Ctrl Pts',(4.9163033542263,0.0603642649825261,4.59402420038378));
#15161=CARTESIAN_POINT('Ctrl Pts',(4.92115458874249,-9.52916733652962E-6,
4.59405847898621));
#15162=CARTESIAN_POINT('Origin',(4.,0.,4.));
#15163=CARTESIAN_POINT('',(5.32884541125756,-1.45357002139801E-5,4.59407911932661));
#15164=CARTESIAN_POINT('',(5.22115458874249,1.46139895546772E-5,4.59411444380891));
#15165=CARTESIAN_POINT('',(4.,-7.27562663373442E-17,4.5941));
#15166=CARTESIAN_POINT('Ctrl Pts',(5.32884541125756,-1.45357002139801E-5,
4.59407911932661));
#15167=CARTESIAN_POINT('Ctrl Pts',(5.32327896849499,0.0692531541268509,
4.59401614001471));
#15168=CARTESIAN_POINT('Ctrl Pts',(5.31771252573242,0.138542285837495,4.5819075943171));
#15169=CARTESIAN_POINT('Ctrl Pts',(5.31214608296985,0.203593590158122,4.55818044906639));
#15170=CARTESIAN_POINT('Ctrl Pts',(5.30419344362604,0.296530782575621,4.5242820624512));
#15171=CARTESIAN_POINT('Ctrl Pts',(5.29624080428224,0.380818089806801,4.46666879957728));
#15172=CARTESIAN_POINT('Ctrl Pts',(5.28828816493843,0.446150240572578,4.39238466650784));
#15173=CARTESIAN_POINT('Ctrl Pts',(5.28033552559462,0.511482391338355,4.3181005334384));
#15174=CARTESIAN_POINT('Ctrl Pts',(5.27238288625081,0.557859385638729,4.22714553017344));
#15175=CARTESIAN_POINT('Ctrl Pts',(5.26443024690701,0.579611004278495,4.13064014464439));
#15176=CARTESIAN_POINT('Ctrl Pts',(5.2564776075632,0.601362622918262,4.03413475911534));
#15177=CARTESIAN_POINT('Ctrl Pts',(5.2485249682194,0.598488865897423,3.93207899132219));
#15178=CARTESIAN_POINT('Ctrl Pts',(5.24057232887559,0.571341089151559,3.8369505488493));
#15179=CARTESIAN_POINT('Ctrl Pts',(5.23261968953179,0.544193312405696,3.74182210637642));
#15180=CARTESIAN_POINT('Ctrl Pts',(5.22466705018798,0.492771515934809,3.65362098922379));
#15181=CARTESIAN_POINT('Ctrl Pts',(5.21671441084417,0.423362714708271,3.58313098523844));
#15182=CARTESIAN_POINT('Ctrl Pts',(5.20876177150037,0.353953913481732,3.51264098125308));
#15183=CARTESIAN_POINT('Ctrl Pts',(5.20080913215656,0.266558107499543,3.45986209043499));
#15184=CARTESIAN_POINT('Ctrl Pts',(5.19285649281275,0.171860624350003,3.43124725102074));
#15185=CARTESIAN_POINT('Ctrl Pts',(5.18490385346895,0.0771631412004631,
3.40263241160649));
#15186=CARTESIAN_POINT('Ctrl Pts',(5.17695121412514,-0.0248360191164267,
3.39818162359609));
#15187=CARTESIAN_POINT('Ctrl Pts',(5.16899857478133,-0.121666070051256,
3.41843905644231));
#15188=CARTESIAN_POINT('Ctrl Pts',(5.16104593543753,-0.218496120986084,
3.43869648928852));
#15189=CARTESIAN_POINT('Ctrl Pts',(5.15309329609372,-0.310157062538852,
3.48366214299137));
#15190=CARTESIAN_POINT('Ctrl Pts',(5.14514065674991,-0.385442096207774,
3.54783835396576));
#15191=CARTESIAN_POINT('Ctrl Pts',(5.13718801740611,-0.460727129876697,
3.61201456494015));
#15192=CARTESIAN_POINT('Ctrl Pts',(5.1292353780623,-0.519636255661773,3.6954013331861));
#15193=CARTESIAN_POINT('Ctrl Pts',(5.1212827387185,-0.554967030609594,3.78780349058054));
#15194=CARTESIAN_POINT('Ctrl Pts',(5.11333009937469,-0.590297805557415,
3.88020564797498));
#15195=CARTESIAN_POINT('Ctrl Pts',(5.10537746003088,-0.60205022966798,3.98162319451792));
#15196=CARTESIAN_POINT('Ctrl Pts',(5.09742482068708,-0.588787409028971,
4.07965645386523));
#15197=CARTESIAN_POINT('Ctrl Pts',(5.08947218134327,-0.575524588389962,
4.17768971321255));
#15198=CARTESIAN_POINT('Ctrl Pts',(5.08151954199946,-0.537246523001379,
4.27233868536424));
#15199=CARTESIAN_POINT('Ctrl Pts',(5.07356690265566,-0.47863322769376,4.35203124438164));
#15200=CARTESIAN_POINT('Ctrl Pts',(5.06561426331185,-0.42001993238614,4.43172380339905));
#15201=CARTESIAN_POINT('Ctrl Pts',(5.05766162396805,-0.341071407159484,
4.49645994928216));
#15202=CARTESIAN_POINT('Ctrl Pts',(5.04970898462424,-0.251440184480074,
4.53832480650817));
#15203=CARTESIAN_POINT('Ctrl Pts',(5.04275446016868,-0.1730583412759,4.5749353153996));
#15204=CARTESIAN_POINT('Ctrl Pts',(5.03579993571312,-0.0865070403179845,
4.59405529558476));
#15205=CARTESIAN_POINT('Ctrl Pts',(5.02884541125756,1.1583539301252E-5,
4.59413174414479));
#15206=CARTESIAN_POINT('Ctrl Pts',(4.92115458874249,-9.52916733652962E-6,
4.59405847898621));
#15207=CARTESIAN_POINT('Ctrl Pts',(4.9242559935701,-0.0386066277022544,
4.59408039337166));
#15208=CARTESIAN_POINT('Ctrl Pts',(4.92735739839772,-0.0771995748988638,
4.59037647703175));
#15209=CARTESIAN_POINT('Ctrl Pts',(4.93045880322533,-0.115049119822012,
4.58290605049323));
#15210=CARTESIAN_POINT('Ctrl Pts',(4.93841144256913,-0.212103131417409,
4.56375034161047));
#15211=CARTESIAN_POINT('Ctrl Pts',(4.94636408191294,-0.304269161635426,
4.51982926360553));
#15212=CARTESIAN_POINT('Ctrl Pts',(4.95431672125675,-0.380278658005779,
4.45651276645759));
#15213=CARTESIAN_POINT('Ctrl Pts',(4.96226936060055,-0.456288154376132,
4.39319626930964));
#15214=CARTESIAN_POINT('Ctrl Pts',(4.97022199994436,-0.516141116898821,
4.31048435301868));
#15215=CARTESIAN_POINT('Ctrl Pts',(4.97817463928816,-0.552519705724467,
4.21848967586497));
#15216=CARTESIAN_POINT('Ctrl Pts',(4.98612727863197,-0.588898294550112,
4.12649499871126));
#15217=CARTESIAN_POINT('Ctrl Pts',(4.99407991797578,-0.601802509678713,
4.0252175606948));
#15218=CARTESIAN_POINT('Ctrl Pts',(5.00203255731958,-0.589654635058918,
3.92703990798411));
#15219=CARTESIAN_POINT('Ctrl Pts',(5.00998519666339,-0.577506760439122,
3.82886225527341));
#15220=CARTESIAN_POINT('Ctrl Pts',(5.0179378360072,-0.540306796070929,3.73378438786847));
#15221=CARTESIAN_POINT('Ctrl Pts',(5.025890475351,-0.482602944251693,3.65343086999412));
#15222=CARTESIAN_POINT('Ctrl Pts',(5.03384311469481,-0.424899092432456,
3.57307735211977));
#15223=CARTESIAN_POINT('Ctrl Pts',(5.04179575403862,-0.346691353162178,
3.50744818377599));
#15224=CARTESIAN_POINT('Ctrl Pts',(5.04974839338242,-0.257541687734669,
3.46456742464414));
#15225=CARTESIAN_POINT('Ctrl Pts',(5.05770103272623,-0.16839202230716,3.42168666551229));
#15226=CARTESIAN_POINT('Ctrl Pts',(5.06565367207003,-0.0683004307224215,
3.40155431559236));
#15227=CARTESIAN_POINT('Ctrl Pts',(5.07360631141384,0.0304955267282049,
3.40663182885918));
#15228=CARTESIAN_POINT('Ctrl Pts',(5.08155895075765,0.129291484178831,3.41170934212599));
#15229=CARTESIAN_POINT('Ctrl Pts',(5.08951159010146,0.226791807495345,3.44199671857955));
#15230=CARTESIAN_POINT('Ctrl Pts',(5.09746422944526,0.311075754224562,3.49379091394262));
#15231=CARTESIAN_POINT('Ctrl Pts',(5.10541686878907,0.395359700953779,3.54558510930568));
#15232=CARTESIAN_POINT('Ctrl Pts',(5.11336950813287,0.466427271095698,3.61888612357825));
#15233=CARTESIAN_POINT('Ctrl Pts',(5.12132214747668,0.515589486279599,3.70473190942573));
#15234=CARTESIAN_POINT('Ctrl Pts',(5.12927478682048,0.564751701463499,3.79057769527322));
#15235=CARTESIAN_POINT('Ctrl Pts',(5.13722742616429,0.592008561689381,3.88896825269562));
#15236=CARTESIAN_POINT('Ctrl Pts',(5.1451800655081,0.594027544563649,3.98787399599556));
#15237=CARTESIAN_POINT('Ctrl Pts',(5.1531327048519,0.596046527437917,4.0867797392955));
#15238=CARTESIAN_POINT('Ctrl Pts',(5.16108534419571,0.572827632960568,4.18620066847299));
#15239=CARTESIAN_POINT('Ctrl Pts',(5.16903798353952,0.527209687216453,4.2739812208502));
#15240=CARTESIAN_POINT('Ctrl Pts',(5.17699062288332,0.481591741472338,4.3617617732274));
#15241=CARTESIAN_POINT('Ctrl Pts',(5.18494326222713,0.413574744461461,4.43790194880433));
#15242=CARTESIAN_POINT('Ctrl Pts',(5.19289590157094,0.331474700441294,4.49309257410834));
#15243=CARTESIAN_POINT('Ctrl Pts',(5.20084854091474,0.24937465642113,4.54828319941234));
#15244=CARTESIAN_POINT('Ctrl Pts',(5.20880118025855,0.153191565391677,4.58252427444343));
#15245=CARTESIAN_POINT('Ctrl Pts',(5.21675381960235,0.0546851202186884,
4.59162936142496));
#15246=CARTESIAN_POINT('Ctrl Pts',(5.21822074264906,0.0365148790664279,
4.59330886194775));
#15247=CARTESIAN_POINT('Ctrl Pts',(5.21968766569578,0.018265586889787,4.59413312238171));
#15248=CARTESIAN_POINT('Ctrl Pts',(5.22115458874249,1.46139895546772E-5,
4.59411444380891));
#15249=CARTESIAN_POINT('Origin',(4.,0.,4.));
#15250=CARTESIAN_POINT('',(5.62884541125756,1.52328526200479E-5,4.59408648697874));
#15251=CARTESIAN_POINT('',(5.52115458874249,-1.55733839743342E-5,4.59409663347568));
#15252=CARTESIAN_POINT('',(4.,-7.27562663373442E-17,4.5941));
#15253=CARTESIAN_POINT('Ctrl Pts',(5.62884541125756,1.52328526200479E-5,
4.59408648697874));
#15254=CARTESIAN_POINT('Ctrl Pts',(5.62666327996447,0.0271682673899915,
4.59411287463303));
#15255=CARTESIAN_POINT('Ctrl Pts',(5.62448114867138,0.054317778225707,4.59228554395034));
#15256=CARTESIAN_POINT('Ctrl Pts',(5.62229901737829,0.0812075234320336,
4.58857548522516));
#15257=CARTESIAN_POINT('Ctrl Pts',(5.61434637803449,0.179205497408217,4.57505441109036));
#15258=CARTESIAN_POINT('Ctrl Pts',(5.60639373869068,0.273753285393806,4.53652709601604));
#15259=CARTESIAN_POINT('Ctrl Pts',(5.59844109934688,0.353291132582354,4.47770402899113));
#15260=CARTESIAN_POINT('Ctrl Pts',(5.59048846000307,0.432828979770902,4.41888096196622));
#15261=CARTESIAN_POINT('Ctrl Pts',(5.58253582065927,0.497356886162411,4.33976214299073));
#15262=CARTESIAN_POINT('Ctrl Pts',(5.57458318131546,0.538985436353474,4.25002092526659));
#15263=CARTESIAN_POINT('Ctrl Pts',(5.56663054197165,0.580613986544537,4.16027970754245));
#15264=CARTESIAN_POINT('Ctrl Pts',(5.55867790262784,0.599343180535155,4.05991609106967));
#15265=CARTESIAN_POINT('Ctrl Pts',(5.55072526328404,0.592883119270616,3.96120089488413));
#15266=CARTESIAN_POINT('Ctrl Pts',(5.54277262394023,0.586423058006077,3.86248569869858));
#15267=CARTESIAN_POINT('Ctrl Pts',(5.53481998459642,0.554773741486382,3.76541892280029));
#15268=CARTESIAN_POINT('Ctrl Pts',(5.52686734525262,0.501804729712613,3.68186830256729));
#15269=CARTESIAN_POINT('Ctrl Pts',(5.51891470590881,0.448835717938844,3.5983176823343));
#15270=CARTESIAN_POINT('Ctrl Pts',(5.51096206656501,0.374547010911001,3.52828321776661));
#15271=CARTESIAN_POINT('Ctrl Pts',(5.5030094272212,0.288021414854312,3.48032757600706));
#15272=CARTESIAN_POINT('Ctrl Pts',(5.4950567878774,0.201495818797622,3.4323719342475));
#15273=CARTESIAN_POINT('Ctrl Pts',(5.48710414853359,0.102733333712086,3.40649511529609));
#15274=CARTESIAN_POINT('Ctrl Pts',(5.47915150918978,0.00380901851787326,
3.40586091270526));
#15275=CARTESIAN_POINT('Ctrl Pts',(5.47119886984597,-0.0951152966763399,
3.40522671011442));
#15276=CARTESIAN_POINT('Ctrl Pts',(5.46324623050217,-0.194201441979227,
3.42983512388417));
#15277=CARTESIAN_POINT('Ctrl Pts',(5.45529359115836,-0.281334786601535,
3.47667744027106));
#15278=CARTESIAN_POINT('Ctrl Pts',(5.44734095181456,-0.368468131223842,
3.52351975665794));
#15279=CARTESIAN_POINT('Ctrl Pts',(5.43938831247075,-0.443648675165568,
3.59259597566196));
#15280=CARTESIAN_POINT('Ctrl Pts',(5.43143567312694,-0.497684572991269,
3.67546058871077));
#15281=CARTESIAN_POINT('Ctrl Pts',(5.42348303378314,-0.551720470816969,
3.75832520175959));
#15282=CARTESIAN_POINT('Ctrl Pts',(5.41553039443933,-0.584611722526643,
3.85497820885321));
#15283=CARTESIAN_POINT('Ctrl Pts',(5.40757775509553,-0.592336924628993,
3.95360246348684));
#15284=CARTESIAN_POINT('Ctrl Pts',(5.39962511575172,-0.600062126731343,
4.05222671812048));
#15285=CARTESIAN_POINT('Ctrl Pts',(5.39167247640791,-0.582621279226368,
4.15282222029412));
#15286=CARTESIAN_POINT('Ctrl Pts',(5.3837198370641,-0.542146763261091,4.24308979978386));
#15287=CARTESIAN_POINT('Ctrl Pts',(5.3757671977203,-0.501672247295815,4.3333573792736));
#15288=CARTESIAN_POINT('Ctrl Pts',(5.36781455837649,-0.438164062870237,
4.41329703607943));
#15289=CARTESIAN_POINT('Ctrl Pts',(5.35986191903269,-0.359386950494509,
4.47313505840055));
#15290=CARTESIAN_POINT('Ctrl Pts',(5.35190927968888,-0.28060983811878,4.53297308072167));
#15291=CARTESIAN_POINT('Ctrl Pts',(5.34395664034507,-0.1865637977929,4.57270946855809));
#15292=CARTESIAN_POINT('Ctrl Pts',(5.33600400100126,-0.0887472388280498,
4.58748590729807));
#15293=CARTESIAN_POINT('Ctrl Pts',(5.33361780442003,-0.0593972924141157,
4.59191959101989));
#15294=CARTESIAN_POINT('Ctrl Pts',(5.3312316078388,-0.0297078841644672,
4.59410611700271));
#15295=CARTESIAN_POINT('Ctrl Pts',(5.32884541125756,-1.45357002139801E-5,
4.59407911932661));
#15296=CARTESIAN_POINT('Ctrl Pts',(5.22115458874249,1.46139895546772E-5,
4.59411444380891));
#15297=CARTESIAN_POINT('Ctrl Pts',(5.22764030503958,-0.0806785298274998,
4.59403186011492));
#15298=CARTESIAN_POINT('Ctrl Pts',(5.23412602133668,-0.161404528346198,
4.57747154641029));
#15299=CARTESIAN_POINT('Ctrl Pts',(5.24061173763377,-0.235476461490165,
4.54549665421293));
#15300=CARTESIAN_POINT('Ctrl Pts',(5.24856437697758,-0.32630179870949,4.50628976108741));
#15301=CARTESIAN_POINT('Ctrl Pts',(5.25651701632139,-0.407122673831612,
4.44390687590439));
#15302=CARTESIAN_POINT('Ctrl Pts',(5.26446965566519,-0.468057634114636,
4.36597515601533));
#15303=CARTESIAN_POINT('Ctrl Pts',(5.272422295009,-0.52899259439766,4.28804343612627));
#15304=CARTESIAN_POINT('Ctrl Pts',(5.28037493435281,-0.570041639841584,
4.19456288153117));
#15305=CARTESIAN_POINT('Ctrl Pts',(5.28832757369661,-0.586185965564114,
4.09696276320888));
#15306=CARTESIAN_POINT('Ctrl Pts',(5.29628021304042,-0.602330291286644,
3.99936264488659));
#15307=CARTESIAN_POINT('Ctrl Pts',(5.30423285238423,-0.59356989728778,3.89764296283709));
#15308=CARTESIAN_POINT('Ctrl Pts',(5.31218549172803,-0.560975861048054,
3.80424033358521));
#15309=CARTESIAN_POINT('Ctrl Pts',(5.32013813107184,-0.528381824808328,
3.71083770433334));
#15310=CARTESIAN_POINT('Ctrl Pts',(5.32809077041564,-0.471954146327742,
3.62575212787907));
#15311=CARTESIAN_POINT('Ctrl Pts',(5.33604340975945,-0.398591877830097,
3.55938647478623));
#15312=CARTESIAN_POINT('Ctrl Pts',(5.34399604910326,-0.325229609332449,
3.49302082169338));
#15313=CARTESIAN_POINT('Ctrl Pts',(5.35194868844707,-0.234932750817741,
3.44537509196196));
#15314=CARTESIAN_POINT('Ctrl Pts',(5.35990132779087,-0.138741323057917,
3.42227462497344));
#15315=CARTESIAN_POINT('Ctrl Pts',(5.36785396713468,-0.042549895298095,
3.39917415798493));
#15316=CARTESIAN_POINT('Ctrl Pts',(5.37580660647848,0.059536101706843,3.40061895373932));
#15317=CARTESIAN_POINT('Ctrl Pts',(5.38375924582229,0.155035264439678,3.42643236627792));
#15318=CARTESIAN_POINT('Ctrl Pts',(5.39171188516609,0.250534427172515,3.45224577881651));
#15319=CARTESIAN_POINT('Ctrl Pts',(5.3996645245099,0.339446755633248,3.5024278081393));
#15320=CARTESIAN_POINT('Ctrl Pts',(5.40761716385371,0.41090150670596,3.57084301769608));
#15321=CARTESIAN_POINT('Ctrl Pts',(5.41556980319751,0.482356257778672,3.63925822725286));
#15322=CARTESIAN_POINT('Ctrl Pts',(5.42352244254132,0.536353431463363,3.72590661704362));
#15323=CARTESIAN_POINT('Ctrl Pts',(5.43147508188513,0.566291137850326,3.82019424128906));
#15324=CARTESIAN_POINT('Ctrl Pts',(5.43942772122893,0.596228844237288,3.91448186553449));
#15325=CARTESIAN_POINT('Ctrl Pts',(5.44738036057274,0.602107083326521,4.01640872423458));
#15326=CARTESIAN_POINT('Ctrl Pts',(5.45533299991655,0.583207160329387,4.11351287069736));
#15327=CARTESIAN_POINT('Ctrl Pts',(5.46328563926035,0.564307237332252,4.21061701716013));
#15328=CARTESIAN_POINT('Ctrl Pts',(5.47123827860416,0.520629152248751,4.30289845138559));
#15329=CARTESIAN_POINT('Ctrl Pts',(5.47919091794796,0.457513145863858,4.37907451119169));
#15330=CARTESIAN_POINT('Ctrl Pts',(5.48714355729177,0.394397139478966,4.45525057099779));
#15331=CARTESIAN_POINT('Ctrl Pts',(5.49509619663558,0.311843211792683,4.51532125638452));
#15332=CARTESIAN_POINT('Ctrl Pts',(5.50304883597938,0.219944704826683,4.5519421079172));
#15333=CARTESIAN_POINT('Ctrl Pts',(5.50908408690042,0.150203009669811,4.5797336395568));
#15334=CARTESIAN_POINT('Ctrl Pts',(5.51511933782146,0.0750795109720808,
4.59401975858331));
#15335=CARTESIAN_POINT('Ctrl Pts',(5.52115458874249,-1.55733839743342E-5,
4.59409663347568));
#15336=CARTESIAN_POINT('Origin',(4.,0.,4.));
#15337=CARTESIAN_POINT('',(5.92884541125757,-1.3134308860685E-5,4.59412454375027));
#15338=CARTESIAN_POINT('',(5.82115458874249,1.31105368646138E-5,4.59407040741879));
#15339=CARTESIAN_POINT('',(4.,-7.27562663373442E-17,4.5941));
#15340=CARTESIAN_POINT('Ctrl Pts',(5.92884541125757,-1.3134308860685E-5,
4.59412454375027));
#15341=CARTESIAN_POINT('Ctrl Pts',(5.92209495209015,0.0839697382976411,
4.5940436242297));
#15342=CARTESIAN_POINT('Ctrl Pts',(5.91534449292274,0.16798613900316,4.57606223573506));
#15343=CARTESIAN_POINT('Ctrl Pts',(5.90859403375532,0.244517407380453,4.54150437939301));
#15344=CARTESIAN_POINT('Ctrl Pts',(5.90064139441152,0.334678026211646,4.50079216098422));
#15345=CARTESIAN_POINT('Ctrl Pts',(5.89268875506771,0.41445008323119,4.43707358099086));
#15346=CARTESIAN_POINT('Ctrl Pts',(5.8847361157239,0.474080337065587,4.35813908232779));
#15347=CARTESIAN_POINT('Ctrl Pts',(5.8767834763801,0.533710590899983,4.27920458366471));
#15348=CARTESIAN_POINT('Ctrl Pts',(5.86883083703629,0.573199041549232,4.18505416633191));
#15349=CARTESIAN_POINT('Ctrl Pts',(5.86087819769249,0.587717699183782,4.08719901244189));
#15350=CARTESIAN_POINT('Ctrl Pts',(5.85292555834868,0.602236356818331,3.98934385855186));
#15351=CARTESIAN_POINT('Ctrl Pts',(5.84497291900487,0.591785221438181,3.88778396810461));
#15352=CARTESIAN_POINT('Ctrl Pts',(5.83702027966107,0.557642080814915,3.79493641494568));
#15353=CARTESIAN_POINT('Ctrl Pts',(5.82906764031726,0.523498940191649,3.70208886178675));
#15354=CARTESIAN_POINT('Ctrl Pts',(5.82111500097346,0.465663794325265,3.61795364591614));
#15355=CARTESIAN_POINT('Ctrl Pts',(5.81316236162965,0.391207780605707,3.55281744653948));
#15356=CARTESIAN_POINT('Ctrl Pts',(5.80520972228584,0.31675176688615,3.48768124716281));
#15357=CARTESIAN_POINT('Ctrl Pts',(5.79725708294203,0.225674885313418,3.44154406428009));
#15358=CARTESIAN_POINT('Ctrl Pts',(5.78930444359823,0.129112523455512,3.42004679519738));
#15359=CARTESIAN_POINT('Ctrl Pts',(5.78135180425442,0.0325501615976049,
3.39854952611466));
#15360=CARTESIAN_POINT('Ctrl Pts',(5.77339916491062,-0.0694976805454773,
3.40169217083197));
#15361=CARTESIAN_POINT('Ctrl Pts',(5.76544652556681,-0.164554263536051,
3.42909049911887));
#15362=CARTESIAN_POINT('Ctrl Pts',(5.75749388622301,-0.259610846526622,
3.45648882740576));
#15363=CARTESIAN_POINT('Ctrl Pts',(5.7495412468792,-0.347676170364685,3.50814283926225));
#15364=CARTESIAN_POINT('Ctrl Pts',(5.74158860753539,-0.417983050247216,
3.57773712775495));
#15365=CARTESIAN_POINT('Ctrl Pts',(5.73363596819158,-0.488289930129746,
3.64733141624764));
#15366=CARTESIAN_POINT('Ctrl Pts',(5.72568332884778,-0.540838366056745,
3.73486598137654));
#15367=CARTESIAN_POINT('Ctrl Pts',(5.71773068950397,-0.569203595796233,
3.82963853060694));
#15368=CARTESIAN_POINT('Ctrl Pts',(5.70977805016017,-0.597568825535722,
3.92441107983734));
#15369=CARTESIAN_POINT('Ctrl Pts',(5.70182541081636,-0.6017508490877,4.02642161316923));
#15370=CARTESIAN_POINT('Ctrl Pts',(5.69387277147255,-0.581238357244447,
4.12319795341528));
#15371=CARTESIAN_POINT('Ctrl Pts',(5.68592013212875,-0.560725865401195,
4.21997429366132));
#15372=CARTESIAN_POINT('Ctrl Pts',(5.67796749278494,-0.515518858162713,
4.31151644082153));
#15373=CARTESIAN_POINT('Ctrl Pts',(5.67001485344113,-0.451144507802385,
4.38663212069642));
#15374=CARTESIAN_POINT('Ctrl Pts',(5.66206221409732,-0.386770157442057,
4.46174780057131));
#15375=CARTESIAN_POINT('Ctrl Pts',(5.65410957475352,-0.303228463959881,
4.52043701316089));
#15376=CARTESIAN_POINT('Ctrl Pts',(5.64615693540972,-0.210733537235404,
4.55552420285805));
#15377=CARTESIAN_POINT('Ctrl Pts',(5.640386427359,-0.143618370026196,4.5809837895275));
#15378=CARTESIAN_POINT('Ctrl Pts',(5.63461591930828,-0.07178924788396,4.59401670649762));
#15379=CARTESIAN_POINT('Ctrl Pts',(5.62884541125756,1.52328526200479E-5,
4.59408648697874));
#15380=CARTESIAN_POINT('Ctrl Pts',(5.52115458874249,-1.55733839743342E-5,
4.59409663347568));
#15381=CARTESIAN_POINT('Ctrl Pts',(5.52307197716526,-0.0238731473664388,
4.59412105649149));
#15382=CARTESIAN_POINT('Ctrl Pts',(5.52498936558803,-0.0477278534282068,
4.59271130989713));
#15383=CARTESIAN_POINT('Ctrl Pts',(5.5269067540108,-0.0714062077139717,
4.58984482465595));
#15384=CARTESIAN_POINT('Ctrl Pts',(5.53485939335461,-0.169615527042917,
4.57795567218339));
#15385=CARTESIAN_POINT('Ctrl Pts',(5.54281203269841,-0.264791079455087,
4.54100634955965));
#15386=CARTESIAN_POINT('Ctrl Pts',(5.55076467204222,-0.345296357402727,
4.48351441471562));
#15387=CARTESIAN_POINT('Ctrl Pts',(5.55871731138603,-0.425801635350366,
4.4260224798716));
#15388=CARTESIAN_POINT('Ctrl Pts',(5.56666995072984,-0.491636638833473,
4.34798793280729));
#15389=CARTESIAN_POINT('Ctrl Pts',(5.57462259007364,-0.534752142022197,
4.2589515597096));
#15390=CARTESIAN_POINT('Ctrl Pts',(5.58257522941745,-0.577867645210921,
4.16991518661191));
#15391=CARTESIAN_POINT('Ctrl Pts',(5.59052786876125,-0.598263648105263,
4.06987698748084));
#15392=CARTESIAN_POINT('Ctrl Pts',(5.59848050810506,-0.59344646156208,3.97106799465478));
#15393=CARTESIAN_POINT('Ctrl Pts',(5.60643314744886,-0.588629275018896,
3.87225900182873));
#15394=CARTESIAN_POINT('Ctrl Pts',(5.61438578679267,-0.558598899038186,
3.77467921530768));
#15395=CARTESIAN_POINT('Ctrl Pts',(5.62233842613648,-0.50702695609161,3.69025909300064));
#15396=CARTESIAN_POINT('Ctrl Pts',(5.63029106548029,-0.455455013145033,
3.6058389706936));
#15397=CARTESIAN_POINT('Ctrl Pts',(5.63824370482409,-0.382341503232591,
3.53457851260056));
#15398=CARTESIAN_POINT('Ctrl Pts',(5.6461963441679,-0.296625548722353,3.48519028027742));
#15399=CARTESIAN_POINT('Ctrl Pts',(5.6541489835117,-0.210909594212113,3.43580204795428));
#15400=CARTESIAN_POINT('Ctrl Pts',(5.66210162285551,-0.112591195104077,
3.40828604140104));
#15401=CARTESIAN_POINT('Ctrl Pts',(5.67005426219932,-0.0136911147678568,
3.40600646716786));
#15402=CARTESIAN_POINT('Ctrl Pts',(5.67800690154312,0.0852089655683624,
3.40372689293467));
#15403=CARTESIAN_POINT('Ctrl Pts',(5.68595954088693,0.184690727132768,3.42668375102154));
#15404=CARTESIAN_POINT('Ctrl Pts',(5.69391218023074,0.272591169676606,3.47207025288287));
#15405=CARTESIAN_POINT('Ctrl Pts',(5.70186481957454,0.360491612220445,3.51745675474419));
#15406=CARTESIAN_POINT('Ctrl Pts',(5.70981745891835,0.436810735743714,3.58527290037998));
#15407=CARTESIAN_POINT('Ctrl Pts',(5.71777009826216,0.492217487918224,3.667227242308));
#15408=CARTESIAN_POINT('Ctrl Pts',(5.72572273760596,0.547624240092733,3.74918158423602));
#15409=CARTESIAN_POINT('Ctrl Pts',(5.73367537694977,0.582118620918482,3.84527412245626));
#15410=CARTESIAN_POINT('Ctrl Pts',(5.74162801629357,0.591483222595687,3.94375623549444));
#15411=CARTESIAN_POINT('Ctrl Pts',(5.74958065563738,0.600847824272892,4.04223834853263));
#15412=CARTESIAN_POINT('Ctrl Pts',(5.75753329498119,0.585082646801554,4.14311003638875));
#15413=CARTESIAN_POINT('Ctrl Pts',(5.76548593432499,0.546115197731279,4.23403836123177));
#15414=CARTESIAN_POINT('Ctrl Pts',(5.7734385736688,0.507147748661005,4.32496668607478));
#15415=CARTESIAN_POINT('Ctrl Pts',(5.78139121301261,0.444978027991796,4.4059516479047));
#15416=CARTESIAN_POINT('Ctrl Pts',(5.78934385235641,0.367207131024688,4.46709173242012));
#15417=CARTESIAN_POINT('Ctrl Pts',(5.79729649170022,0.28943623405758,4.52823181693554));
#15418=CARTESIAN_POINT('Ctrl Pts',(5.80524913104403,0.196064160792572,4.56952702413646));
#15419=CARTESIAN_POINT('Ctrl Pts',(5.81320177038783,0.0985069184831505,
4.58592845199323));
#15420=CARTESIAN_POINT('Ctrl Pts',(5.81585270983939,0.0659871057213339,
4.59139571767544));
#15421=CARTESIAN_POINT('Ctrl Pts',(5.81850364929094,0.0330022532417819,
4.59409688335147));
#15422=CARTESIAN_POINT('Ctrl Pts',(5.82115458874249,1.31105368646138E-5,
4.59407040741879));
#15423=CARTESIAN_POINT('Origin',(4.,0.,4.));
#15424=CARTESIAN_POINT('',(6.22884541125756,-1.27841859475647E-5,4.5940334609955));
#15425=CARTESIAN_POINT('',(6.12115458874249,-9.50793186244619E-6,4.59413936148612));
#15426=CARTESIAN_POINT('',(4.,-7.27562663373442E-17,4.5941));
#15427=CARTESIAN_POINT('Ctrl Pts',(6.22884541125756,-1.27841859475647E-5,
4.5940334609955));
#15428=CARTESIAN_POINT('Ctrl Pts',(6.22547926355963,0.0418951881409122,
4.59406590912705));
#15429=CARTESIAN_POINT('Ctrl Pts',(6.2221131158617,0.0838018877146867,4.58971510200585));
#15430=CARTESIAN_POINT('Ctrl Pts',(6.21874696816377,0.124749109322564,4.58093223526196));
#15431=CARTESIAN_POINT('Ctrl Pts',(6.21079432881996,0.22148832423537,4.56018241146135));
#15432=CARTESIAN_POINT('Ctrl Pts',(6.20284168947616,0.31287214740051,4.51469474440412));
#15433=CARTESIAN_POINT('Ctrl Pts',(6.19488905013236,0.387808805213989,4.4501133836823));
#15434=CARTESIAN_POINT('Ctrl Pts',(6.18693641078855,0.462745463027469,4.38553202296047));
#15435=CARTESIAN_POINT('Ctrl Pts',(6.17898377144474,0.521234955489287,4.30185696857405));
#15436=CARTESIAN_POINT('Ctrl Pts',(6.17103113210093,0.556083161424236,4.20927485003939));
#15437=CARTESIAN_POINT('Ctrl Pts',(6.16307849275713,0.590931367359184,4.11669273150472));
#15438=CARTESIAN_POINT('Ctrl Pts',(6.15512585341332,0.602138286767263,4.0152035488218));
#15439=CARTESIAN_POINT('Ctrl Pts',(6.14717321406952,0.588356486924291,3.9172389266648));
#15440=CARTESIAN_POINT('Ctrl Pts',(6.13922057472571,0.574574687081318,3.81927430450779));
#15441=CARTESIAN_POINT('Ctrl Pts',(6.1312679353819,0.535804167987293,3.7248342428767));
#15442=CARTESIAN_POINT('Ctrl Pts',(6.12331529603809,0.476773096629474,3.64545304401991));
#15443=CARTESIAN_POINT('Ctrl Pts',(6.11536265669429,0.417742025271657,3.56607184516312));
#15444=CARTESIAN_POINT('Ctrl Pts',(6.10741001735048,0.338450401650047,3.50174950908064));
#15445=CARTESIAN_POINT('Ctrl Pts',(6.09945737800668,0.248599092144812,3.46035682177302));
#15446=CARTESIAN_POINT('Ctrl Pts',(6.09150473866287,0.158747782639575,3.41896413446539));
#15447=CARTESIAN_POINT('Ctrl Pts',(6.08355209931906,0.0583367872507115,
3.40050109593262));
#15448=CARTESIAN_POINT('Ctrl Pts',(6.07559945997526,-0.0403606640336046,
3.40722161935946));
#15449=CARTESIAN_POINT('Ctrl Pts',(6.06764682063145,-0.139058115317921,
3.4139421427863));
#15450=CARTESIAN_POINT('Ctrl Pts',(6.05969418128764,-0.23604202249769,3.44584622817275));
#15451=CARTESIAN_POINT('Ctrl Pts',(6.05174154194384,-0.319452991027635,
3.49903499090221));
#15452=CARTESIAN_POINT('Ctrl Pts',(6.04378890260003,-0.40286395955758,3.55222375363166));
#15453=CARTESIAN_POINT('Ctrl Pts',(6.03583626325623,-0.472701989437702,
3.62669719370411));
#15454=CARTESIAN_POINT('Ctrl Pts',(6.02788362391242,-0.520429378860104,
3.71334895258148));
#15455=CARTESIAN_POINT('Ctrl Pts',(6.01993098456861,-0.568156768282506,
3.80000071145885));
#15456=CARTESIAN_POINT('Ctrl Pts',(6.0119783452248,-0.593773517247188,3.89883078914114));
#15457=CARTESIAN_POINT('Ctrl Pts',(6.004025705881,-0.594147126960238,3.99775637428654));
#15458=CARTESIAN_POINT('Ctrl Pts',(5.99607306653719,-0.594520736673288,
4.09668195943193));
#15459=CARTESIAN_POINT('Ctrl Pts',(5.98812042719339,-0.569651207134705,
4.19570305204043));
#15460=CARTESIAN_POINT('Ctrl Pts',(5.98016778784958,-0.52257944308796,4.28271270390554));
#15461=CARTESIAN_POINT('Ctrl Pts',(5.97221514850578,-0.475507679041215,
4.36972235577065));
#15462=CARTESIAN_POINT('Ctrl Pts',(5.96426250916196,-0.406233680486307,
4.44472056689237));
#15463=CARTESIAN_POINT('Ctrl Pts',(5.95630986981816,-0.323226996343023,
4.49853792802592));
#15464=CARTESIAN_POINT('Ctrl Pts',(5.94835723047435,-0.240220312199739,
4.55235528915947));
#15465=CARTESIAN_POINT('Ctrl Pts',(5.94040459113055,-0.143480942468078,
4.58499180030486));
#15466=CARTESIAN_POINT('Ctrl Pts',(5.93245195178675,-0.0448366672808267,
4.59245712746544));
#15467=CARTESIAN_POINT('Ctrl Pts',(5.93124977161035,-0.0299248641651563,
4.59358564190382));
#15468=CARTESIAN_POINT('Ctrl Pts',(5.93004759143396,-0.0149695309183627,
4.59413895459864));
#15469=CARTESIAN_POINT('Ctrl Pts',(5.92884541125757,-1.3134308860685E-5,
4.59412454375027));
#15470=CARTESIAN_POINT('Ctrl Pts',(5.82115458874249,1.31105368646138E-5,
4.59407040741879));
#15471=CARTESIAN_POINT('Ctrl Pts',(5.82645628863475,-0.0659629472043463,
4.59401745734129));
#15472=CARTESIAN_POINT('Ctrl Pts',(5.831757988527,-0.131956164688202,4.58305467757793));
#15473=CARTESIAN_POINT('Ctrl Pts',(5.83705968841925,-0.194280919321303,
4.56148970414564));
#15474=CARTESIAN_POINT('Ctrl Pts',(5.84501232776306,-0.287769103462499,
4.52914187992864));
#15475=CARTESIAN_POINT('Ctrl Pts',(5.85296496710686,-0.373003060391055,
4.47293858298203));
#15476=CARTESIAN_POINT('Ctrl Pts',(5.86091760645067,-0.439561779454174,
4.39975142997742));
#15477=CARTESIAN_POINT('Ctrl Pts',(5.86887024579447,-0.506120498517293,
4.32656427697281));
#15478=CARTESIAN_POINT('Ctrl Pts',(5.87682288513828,-0.554003979714975,
4.2363932679102));
#15479=CARTESIAN_POINT('Ctrl Pts',(5.88477552448209,-0.577357812582609,
4.14026304025204));
#15480=CARTESIAN_POINT('Ctrl Pts',(5.8927281638259,-0.600711645450243,4.04413281259387));
#15481=CARTESIAN_POINT('Ctrl Pts',(5.9006808031697,-0.59953582998783,3.94204336634015));
#15482=CARTESIAN_POINT('Ctrl Pts',(5.90863344251351,-0.573974130801472,
3.84647652011691));
#15483=CARTESIAN_POINT('Ctrl Pts',(5.91658608185731,-0.548412431615114,
3.75090967389367));
#15484=CARTESIAN_POINT('Ctrl Pts',(5.92453872120112,-0.498464848704808,
3.66186542770092));
#15485=CARTESIAN_POINT('Ctrl Pts',(5.93249136054493,-0.430238144626613,
3.59023066587279));
#15486=CARTESIAN_POINT('Ctrl Pts',(5.94044399988873,-0.362011440548417,
3.51859590404466));
#15487=CARTESIAN_POINT('Ctrl Pts',(5.94839663923254,-0.275505615302329,
3.46437062658116));
#15488=CARTESIAN_POINT('Ctrl Pts',(5.95634927857635,-0.181297202577209,
3.43418458862315));
#15489=CARTESIAN_POINT('Ctrl Pts',(5.96430191792015,-0.087088789852092,
3.40399855066514));
#15490=CARTESIAN_POINT('Ctrl Pts',(5.97225455726396,0.0148222103520573,
3.39785175221263));
#15491=CARTESIAN_POINT('Ctrl Pts',(5.98020719660777,0.111975824940657,3.41649576758492));
#15492=CARTESIAN_POINT('Ctrl Pts',(5.98815983595157,0.209129439529257,3.43513978295721));
#15493=CARTESIAN_POINT('Ctrl Pts',(5.99611247529537,0.301525668502307,3.47857461215431));
#15494=CARTESIAN_POINT('Ctrl Pts',(6.00406511463918,0.377867748972965,3.54148967172874));
#15495=CARTESIAN_POINT('Ctrl Pts',(6.01201775398299,0.454209829443624,3.60440473130317));
#15496=CARTESIAN_POINT('Ctrl Pts',(6.0199703933268,0.514497761411887,3.68680002125492));
#15497=CARTESIAN_POINT('Ctrl Pts',(6.02792303267061,0.551360647735685,3.77860175380959));
#15498=CARTESIAN_POINT('Ctrl Pts',(6.03587567201441,0.588223534059482,3.87040348636426));
#15499=CARTESIAN_POINT('Ctrl Pts',(6.04382831135821,0.601661374738811,3.97161166152184));
#15500=CARTESIAN_POINT('Ctrl Pts',(6.05178095070202,0.590030977261751,4.06985190192822));
#15501=CARTESIAN_POINT('Ctrl Pts',(6.05973359004583,0.578400579784692,4.16809214233459));
#15502=CARTESIAN_POINT('Ctrl Pts',(6.06768622938964,0.541701944151245,4.26336444798975));
#15503=CARTESIAN_POINT('Ctrl Pts',(6.07563886873345,0.484422419230229,4.3440210474869));
#15504=CARTESIAN_POINT('Ctrl Pts',(6.08359150807725,0.427142894309213,4.42467764698404));
#15505=CARTESIAN_POINT('Ctrl Pts',(6.09154414742105,0.349282480100627,4.49071854032316));
#15506=CARTESIAN_POINT('Ctrl Pts',(6.09949678676486,0.26035984028865,4.53406826097581));
#15507=CARTESIAN_POINT('Ctrl Pts',(6.10671605409073,0.179637418414302,4.5734203814938));
#15508=CARTESIAN_POINT('Ctrl Pts',(6.11393532141662,0.0897989573399868,
4.59407340590587));
#15509=CARTESIAN_POINT('Ctrl Pts',(6.12115458874249,-9.50793186244619E-6,
4.59413936148612));
#15510=CARTESIAN_POINT('Origin',(4.,0.,4.));
#15511=CARTESIAN_POINT('',(6.52884541125757,2.61457539729726E-5,4.59508370962656));
#15512=CARTESIAN_POINT('',(6.42115458874249,-0.000630941829811112,4.59394485456974));
#15513=CARTESIAN_POINT('',(4.,-7.27562663373442E-17,4.5941));
#15514=CARTESIAN_POINT('Ctrl Pts',(6.52884541125757,2.61457539729726E-5,
4.59508370962656));
#15515=CARTESIAN_POINT('Ctrl Pts',(6.5129582963415,0.196771080344787,4.59506033873941));
#15516=CARTESIAN_POINT('Ctrl Pts',(6.49707118142544,0.393450480974957,4.48779253427891));
#15517=CARTESIAN_POINT('Ctrl Pts',(6.48118406650938,0.500111739713094,4.32240987211318));
#15518=CARTESIAN_POINT('Ctrl Pts',(6.46527878782176,0.606894944490356,4.15683812760557));
#15519=CARTESIAN_POINT('Ctrl Pts',(6.44937350913416,0.623454053851315,3.93301856375293));
#15520=CARTESIAN_POINT('Ctrl Pts',(6.43346823044654,0.541809843535619,3.75368369989414));
#15521=CARTESIAN_POINT('Ctrl Pts',(6.41756295175893,0.460165633219924,3.57434883603535));
#15522=CARTESIAN_POINT('Ctrl Pts',(6.40165767307132,0.280318103227576,3.43949867217041));
#15523=CARTESIAN_POINT('Ctrl Pts',(6.3857523943837,0.085604811340831,3.41110814665827));
#15524=CARTESIAN_POINT('Ctrl Pts',(6.36984711569609,-0.109108480545914,
3.38271762114613));
#15525=CARTESIAN_POINT('Ctrl Pts',(6.35394183700848,-0.318687534327053,
3.46078673398678));
#15526=CARTESIAN_POINT('Ctrl Pts',(6.33803655832087,-0.448733343985475,
3.60951691634857));
#15527=CARTESIAN_POINT('Ctrl Pts',(6.33008391897706,-0.513756248814686,
3.68388200752946));
#15528=CARTESIAN_POINT('Ctrl Pts',(6.32213127963325,-0.558895842613217,
3.77591236609064));
#15529=CARTESIAN_POINT('Ctrl Pts',(6.31417864028945,-0.579995970841135,
3.87270290659392));
#15530=CARTESIAN_POINT('Ctrl Pts',(6.30622600094564,-0.601096099069052,
3.9694934470972));
#15531=CARTESIAN_POINT('Ctrl Pts',(6.29827336160184,-0.598156761726356,
4.07104416954258));
#15532=CARTESIAN_POINT('Ctrl Pts',(6.29032072225803,-0.570614590620327,
4.16591643177432));
#15533=CARTESIAN_POINT('Ctrl Pts',(6.28236808291422,-0.543072419514299,
4.26078869400605));
#15534=CARTESIAN_POINT('Ctrl Pts',(6.27441544357042,-0.490927414644939,
4.34898249602413));
#15535=CARTESIAN_POINT('Ctrl Pts',(6.26646280422661,-0.421087730399527,
4.41916768405122));
#15536=CARTESIAN_POINT('Ctrl Pts',(6.2585101648828,-0.351248046154114,4.48935287207832));
#15537=CARTESIAN_POINT('Ctrl Pts',(6.250557525539,-0.263713682532649,4.54152944611444));
#15538=CARTESIAN_POINT('Ctrl Pts',(6.24260488619519,-0.168899197391682,
4.5696117428605));
#15539=CARTESIAN_POINT('Ctrl Pts',(6.23801839454932,-0.114217245248871,
4.58580752565092));
#15540=CARTESIAN_POINT('Ctrl Pts',(6.23343190290344,-0.0571138332845632,
4.59398924930378));
#15541=CARTESIAN_POINT('Ctrl Pts',(6.22884541125756,-1.27841859475647E-5,
4.5940334609955));
#15542=CARTESIAN_POINT('Ctrl Pts',(6.12115458874249,-9.50793186244619E-6,
4.59413936148612));
#15543=CARTESIAN_POINT('Ctrl Pts',(6.12188796076042,-0.00913273504488762,
4.59414606160884));
#15544=CARTESIAN_POINT('Ctrl Pts',(6.12262133277835,-0.0182556526135436,
4.59394031163173));
#15545=CARTESIAN_POINT('Ctrl Pts',(6.12335470479628,-0.0273686726716501,
4.59352013235631));
#15546=CARTESIAN_POINT('Ctrl Pts',(6.13130734414009,-0.126189680404606,
4.58896373511797));
#15547=CARTESIAN_POINT('Ctrl Pts',(6.13925998348389,-0.223846830455152,
4.55919239267511));
#15548=CARTESIAN_POINT('Ctrl Pts',(6.14721262282769,-0.308403173896691,
4.50784224986958));
#15549=CARTESIAN_POINT('Ctrl Pts',(6.1551652621715,-0.392959517338232,4.45649210706404));
#15550=CARTESIAN_POINT('Ctrl Pts',(6.16311790151532,-0.464415054170765,
4.38356316389581));
#15551=CARTESIAN_POINT('Ctrl Pts',(6.17107054085912,-0.514027768136376,
4.29797916579711));
#15552=CARTESIAN_POINT('Ctrl Pts',(6.17902318020293,-0.563640482101988,
4.2123951676984));
#15553=CARTESIAN_POINT('Ctrl Pts',(6.18697581954673,-0.591410373200678,
4.11415611466921));
#15554=CARTESIAN_POINT('Ctrl Pts',(6.19492845889053,-0.593952774873424,
4.0152594949342));
#15555=CARTESIAN_POINT('Ctrl Pts',(6.20288109823434,-0.59649517654617,3.9163628751992));
#15556=CARTESIAN_POINT('Ctrl Pts',(6.21083373757815,-0.573810088792972,
3.81680868875837));
#15557=CARTESIAN_POINT('Ctrl Pts',(6.21878637692196,-0.528651094032059,
3.72879442104321));
#15558=CARTESIAN_POINT('Ctrl Pts',(6.22673901626577,-0.483492099271145,
3.64078015332805));
#15559=CARTESIAN_POINT('Ctrl Pts',(6.23469165560957,-0.415859197502516,
3.56430580433857));
#15560=CARTESIAN_POINT('Ctrl Pts',(6.24264429495337,-0.334059153459168,
3.50867301156809));
#15561=CARTESIAN_POINT('Ctrl Pts',(6.25059693429718,-0.252259109415819,
3.45304021879761));
#15562=CARTESIAN_POINT('Ctrl Pts',(6.25854957364099,-0.156291923097747,
3.41824898224614));
#15563=CARTESIAN_POINT('Ctrl Pts',(6.2665022129848,-0.057819682214149,3.40864436538418));
#15564=CARTESIAN_POINT('Ctrl Pts',(6.2744548523286,0.0406525586694487,3.39903974852221));
#15565=CARTESIAN_POINT('Ctrl Pts',(6.28240749167241,0.141629854118573,3.41462175134974));
#15566=CARTESIAN_POINT('Ctrl Pts',(6.29036013101621,0.232632044389671,3.453312878872));
#15567=CARTESIAN_POINT('Ctrl Pts',(6.29831277036002,0.323634234660771,3.49200400639426));
#15568=CARTESIAN_POINT('Ctrl Pts',(6.30626540970382,0.404661319753841,3.55380425861124));
#15569=CARTESIAN_POINT('Ctrl Pts',(6.31421804904763,0.466059055789261,3.63148218419904));
#15570=CARTESIAN_POINT('Ctrl Pts',(6.32217068839144,0.527456791824679,3.70916010978684));
#15571=CARTESIAN_POINT('Ctrl Pts',(6.33012332773525,0.569225178802449,3.80271570874544));
#15572=CARTESIAN_POINT('Ctrl Pts',(6.33807596707905,0.585790493249255,3.90010619949006));
#15573=CARTESIAN_POINT('Ctrl Pts',(6.34602860642286,0.602355807696062,3.99749669023468));
#15574=CARTESIAN_POINT('Ctrl Pts',(6.35398124576666,0.593718049611903,4.09872207276531));
#15575=CARTESIAN_POINT('Ctrl Pts',(6.36193388511047,0.56173881546021,4.19248215342453));
#15576=CARTESIAN_POINT('Ctrl Pts',(6.36988652445427,0.529759581308516,4.28624223408375));
#15577=CARTESIAN_POINT('Ctrl Pts',(6.37783916379808,0.474438871089287,4.37253701287156));
#15578=CARTESIAN_POINT('Ctrl Pts',(6.38579180314189,0.401374624788453,4.4390182948332));
#15579=CARTESIAN_POINT('Ctrl Pts',(6.39757939834209,0.293077024234899,4.53755846574697));
#15580=CARTESIAN_POINT('Ctrl Pts',(6.40936699354229,0.145797072855576,4.59256860517148));
#15581=CARTESIAN_POINT('Ctrl Pts',(6.42115458874249,-0.000630941829811112,
4.59394485456974));
#15582=CARTESIAN_POINT('Origin',(4.,0.,4.));
#15583=CARTESIAN_POINT('',(6.82884541125756,0.000528213615369061,4.5937871332276));
#15584=CARTESIAN_POINT('',(6.72115458874249,0.000109070110168276,4.59505938903171));
#15585=CARTESIAN_POINT('',(4.,-7.27562663373442E-17,4.5941));
#15586=CARTESIAN_POINT('Ctrl Pts',(6.82884541125756,0.000528213615369061,
4.5937871332276));
#15587=CARTESIAN_POINT('Ctrl Pts',(6.82429524715479,0.0572034606387535,
4.59426930340541));
#15588=CARTESIAN_POINT('Ctrl Pts',(6.81974508305202,0.113754426020979,4.58681959872387));
#15589=CARTESIAN_POINT('Ctrl Pts',(6.81519491894924,0.167823213394864,4.57092612439125));
#15590=CARTESIAN_POINT('Ctrl Pts',(6.79928964026163,0.356822799356826,4.51536985589957));
#15591=CARTESIAN_POINT('Ctrl Pts',(6.78338436157403,0.515493156338912,4.35664088088147));
#15592=CARTESIAN_POINT('Ctrl Pts',(6.76747908288642,0.570983871223461,4.16762126762428));
#15593=CARTESIAN_POINT('Ctrl Pts',(6.7515738041988,0.626474586108011,3.97860165436708));
#15594=CARTESIAN_POINT('Ctrl Pts',(6.73566852551118,0.578785658895023,3.75929140287077));
#15595=CARTESIAN_POINT('Ctrl Pts',(6.71976324682357,0.449805704301045,3.61038767491097));
#15596=CARTESIAN_POINT('Ctrl Pts',(6.70385796813595,0.320825749707067,3.46148394695116));
#15597=CARTESIAN_POINT('Ctrl Pts',(6.68795268944834,0.110554767732096,3.38298674252784));
#15598=CARTESIAN_POINT('Ctrl Pts',(6.67204741076073,-0.0844443642884844,
3.4109402193496));
#15599=CARTESIAN_POINT('Ctrl Pts',(6.65614213207312,-0.279443496309066,
3.43889369617135));
#15600=CARTESIAN_POINT('Ctrl Pts',(6.64023685338551,-0.459170778375258,
3.57329785423817));
#15601=CARTESIAN_POINT('Ctrl Pts',(6.6243315746979,-0.541132009270427,3.75243704050979));
#15602=CARTESIAN_POINT('Ctrl Pts',(6.60842629601029,-0.623093240165596,
3.9315762267814));
#15603=CARTESIAN_POINT('Ctrl Pts',(6.59252101732267,-0.60728841988974,4.15545044125781));
#15604=CARTESIAN_POINT('Ctrl Pts',(6.57661573863506,-0.500919754058047,
4.32127168369798));
#15605=CARTESIAN_POINT('Ctrl Pts',(6.56069229617589,-0.394429615589227,
4.48728229340579));
#15606=CARTESIAN_POINT('Ctrl Pts',(6.54476885371673,-0.197168666623305,
4.59510713395368));
#15607=CARTESIAN_POINT('Ctrl Pts',(6.52884541125757,2.61457539729726E-5,
4.59508370962656));
#15608=CARTESIAN_POINT('Ctrl Pts',(6.42115458874249,-0.000630941829811112,
4.59394485456974));
#15609=CARTESIAN_POINT('Ctrl Pts',(6.4252722722299,-0.0517816819022344,
4.59442561076518));
#15610=CARTESIAN_POINT('Ctrl Pts',(6.42938995571731,-0.102828462800867,
4.58836159088269));
#15611=CARTESIAN_POINT('Ctrl Pts',(6.43350763920472,-0.152073274319339,
4.5753220992581));
#15612=CARTESIAN_POINT('Ctrl Pts',(6.44941291789233,-0.342290043897387,
4.52495476314113));
#15613=CARTESIAN_POINT('Ctrl Pts',(6.46531819657995,-0.5056209461254,4.37051151428857));
#15614=CARTESIAN_POINT('Ctrl Pts',(6.48122347526756,-0.56632363157735,4.18304963962536));
#15615=CARTESIAN_POINT('Ctrl Pts',(6.49712875395518,-0.627026317029301,
3.99558776496215));
#15616=CARTESIAN_POINT('Ctrl Pts',(6.51303403264279,-0.58510078570519,3.77510726448829));
#15617=CARTESIAN_POINT('Ctrl Pts',(6.5289393113304,-0.460166914262479,3.62276494217392));
#15618=CARTESIAN_POINT('Ctrl Pts',(6.54484459001801,-0.335233042819767,
3.47042261985956));
#15619=CARTESIAN_POINT('Ctrl Pts',(6.56074986870563,-0.127290831258456,
3.38621847570468));
#15620=CARTESIAN_POINT('Ctrl Pts',(6.57665514739324,0.068373869747762,3.4088573345089));
#15621=CARTESIAN_POINT('Ctrl Pts',(6.59256042608085,0.26403857075398,3.43149619331313));
#15622=CARTESIAN_POINT('Ctrl Pts',(6.60846570476847,0.447425761205104,3.56097805507645));
#15623=CARTESIAN_POINT('Ctrl Pts',(6.62437098345608,0.534230294511761,3.73782813427527));
#15624=CARTESIAN_POINT('Ctrl Pts',(6.64027626214369,0.621034827818418,3.91467821347409));
#15625=CARTESIAN_POINT('Ctrl Pts',(6.65618154083131,0.611256703980608,4.1388965101084));
#15626=CARTESIAN_POINT('Ctrl Pts',(6.67208681951892,0.509439333868548,4.30754322537844));
#15627=CARTESIAN_POINT('Ctrl Pts',(6.68799209820653,0.40762196375649,4.47618994064847));
#15628=CARTESIAN_POINT('Ctrl Pts',(6.70389737689414,0.213765347370184,4.58926507455422));
#15629=CARTESIAN_POINT('Ctrl Pts',(6.71980265558175,0.016851802420978,4.59484308232941));
#15630=CARTESIAN_POINT('Ctrl Pts',(6.72025329996867,0.0112726493937942,
4.59500112406784));
#15631=CARTESIAN_POINT('Ctrl Pts',(6.72070394435558,0.00569104238866241,
4.59507287148453));
#15632=CARTESIAN_POINT('Ctrl Pts',(6.72115458874249,0.000109070110168276,
4.59505938903171));
#15633=CARTESIAN_POINT('Origin',(4.,0.,4.));
#15634=CARTESIAN_POINT('',(7.12884541125757,-0.000233413975479213,4.59320261234329));
#15635=CARTESIAN_POINT('',(7.02115458874249,0.000491936389841303,4.5936290357477));
#15636=CARTESIAN_POINT('',(4.,-7.27562663373442E-17,4.5941));
#15637=CARTESIAN_POINT('Ctrl Pts',(7.12884541125757,-0.000233413975479213,
4.59320261234329));
#15638=CARTESIAN_POINT('Ctrl Pts',(7.11972691928047,0.113624805666132,4.59280158872514));
#15639=CARTESIAN_POINT('Ctrl Pts',(7.11060842730338,0.227688545642871,4.56127879346404));
#15640=CARTESIAN_POINT('Ctrl Pts',(7.10148993532628,0.322592019514134,4.50005536307953));
#15641=CARTESIAN_POINT('Ctrl Pts',(7.08558465663867,0.488131036726243,4.39326405099382));
#15642=CARTESIAN_POINT('Ctrl Pts',(7.06967937795105,0.595374147168556,4.19610732087965));
#15643=CARTESIAN_POINT('Ctrl Pts',(7.05377409926343,0.595079946532544,3.99911121186167));
#15644=CARTESIAN_POINT('Ctrl Pts',(7.03786882057582,0.594785745896532,3.80211510284369));
#15645=CARTESIAN_POINT('Ctrl Pts',(7.02196354188821,0.486954234182196,3.60527961492189));
#15646=CARTESIAN_POINT('Ctrl Pts',(7.0060582632006,0.321096900356496,3.49898325846904));
#15647=CARTESIAN_POINT('Ctrl Pts',(6.99015298451299,0.155239566530797,3.3926869020162));
#15648=CARTESIAN_POINT('Ctrl Pts',(6.97424770582538,-0.0686435894062663,
3.37692967703231));
#15649=CARTESIAN_POINT('Ctrl Pts',(6.95834242713776,-0.247754555527299,
3.45894666907189));
#15650=CARTESIAN_POINT('Ctrl Pts',(6.94243714845015,-0.426865521648332,
3.54096366111146));
#15651=CARTESIAN_POINT('Ctrl Pts',(6.92653186976253,-0.561204297953336,
3.72075487017451));
#15652=CARTESIAN_POINT('Ctrl Pts',(6.91062659107492,-0.589088840804576,
3.91576771430201));
#15653=CARTESIAN_POINT('Ctrl Pts',(6.89472131238731,-0.616973383655816,
4.11078055842951));
#15654=CARTESIAN_POINT('Ctrl Pts',(6.8788160336997,-0.538403693053295,4.32101503762147));
#15655=CARTESIAN_POINT('Ctrl Pts',(6.86291075501209,-0.389454440281117,
4.44994049623482));
#15656=CARTESIAN_POINT('Ctrl Pts',(6.85155564042725,-0.283116420949728,
4.54198310574898));
#15657=CARTESIAN_POINT('Ctrl Pts',(6.8402005258424,-0.140907108175025,4.59258385846765));
#15658=CARTESIAN_POINT('Ctrl Pts',(6.82884541125756,0.000528213615369061,
4.5937871332276));
#15659=CARTESIAN_POINT('Ctrl Pts',(6.72115458874249,0.000109070110168276,
4.59505938903171));
#15660=CARTESIAN_POINT('Ctrl Pts',(6.73660922304319,-0.191322006690816,
4.59459701474307));
#15661=CARTESIAN_POINT('Ctrl Pts',(6.75206385734389,-0.38318268672033,4.49389457135631));
#15662=CARTESIAN_POINT('Ctrl Pts',(6.76751849164459,-0.49122657597837,4.33588597251985));
#15663=CARTESIAN_POINT('Ctrl Pts',(6.78342377033221,-0.60242093591639,4.17326997329048));
#15664=CARTESIAN_POINT('Ctrl Pts',(6.79932904901982,-0.624839182280325,
3.94995709318712));
#15665=CARTESIAN_POINT('Ctrl Pts',(6.81523432770743,-0.548195780923551,
3.76848141254984));
#15666=CARTESIAN_POINT('Ctrl Pts',(6.83113960639504,-0.471552379566775,
3.58700573191256));
#15667=CARTESIAN_POINT('Ctrl Pts',(6.84704488508266,-0.295847330489284,
3.44736725074137));
#15668=CARTESIAN_POINT('Ctrl Pts',(6.86295016377027,-0.101752734572189,
3.41368297698799));
#15669=CARTESIAN_POINT('Ctrl Pts',(6.87885544245788,0.0923418613449005,
3.37999870323461));
#15670=CARTESIAN_POINT('Ctrl Pts',(6.8947607211455,0.304826004101594,3.45226863689903));
#15671=CARTESIAN_POINT('Ctrl Pts',(6.91066599983311,0.438133727661537,3.59730899203965));
#15672=CARTESIAN_POINT('Ctrl Pts',(6.92657127852072,0.571441451221483,3.74234934718029));
#15673=CARTESIAN_POINT('Ctrl Pts',(6.94247655720833,0.625572755584675,3.96016012379713));
#15674=CARTESIAN_POINT('Ctrl Pts',(6.95838183589594,0.57567402069499,4.15073208753033));
#15675=CARTESIAN_POINT('Ctrl Pts',(6.97428711458356,0.525775285805305,4.34130405126353));
#15676=CARTESIAN_POINT('Ctrl Pts',(6.99019239327118,0.371846511662747,4.5046372021131));
#15677=CARTESIAN_POINT('Ctrl Pts',(7.00609767195879,0.184564651688987,4.56573572985967));
#15678=CARTESIAN_POINT('Ctrl Pts',(7.01111664422002,0.125467135782336,4.58501560681028));
#15679=CARTESIAN_POINT('Ctrl Pts',(7.01613561648126,0.0630485115161635,
4.59411554829291));
#15680=CARTESIAN_POINT('Ctrl Pts',(7.02115458874249,0.000491936389841303,
4.5936290357477));
#15681=CARTESIAN_POINT('Origin',(4.,0.,4.));
#15682=CARTESIAN_POINT('',(7.42884541125756,-0.000438237927964824,4.59464495791636));
#15683=CARTESIAN_POINT('',(7.32115458874249,-0.000317338366111653,4.59328419319629));
#15684=CARTESIAN_POINT('',(4.,-7.27562663373442E-17,4.5941));
#15685=CARTESIAN_POINT('Ctrl Pts',(7.42884541125756,-0.000438237927964824,
4.59464495791636));
#15686=CARTESIAN_POINT('Ctrl Pts',(7.41515859140615,0.169409178821721,4.5932420274804));
#15687=CARTESIAN_POINT('Ctrl Pts',(7.40147177155473,0.340360224580004,4.51673272682389));
#15688=CARTESIAN_POINT('Ctrl Pts',(7.38778495170331,0.450965110664874,4.38826722161738));
#15689=CARTESIAN_POINT('Ctrl Pts',(7.37187967301569,0.579497637321094,4.23897909740477));
#15690=CARTESIAN_POINT('Ctrl Pts',(7.35597439432808,0.626535888751401,4.01952688559808));
#15691=CARTESIAN_POINT('Ctrl Pts',(7.34006911564046,0.570481892017836,3.83067375781486));
#15692=CARTESIAN_POINT('Ctrl Pts',(7.32416383695285,0.51442789528427,3.64182063003164));
#15693=CARTESIAN_POINT('Ctrl Pts',(7.30825855826524,0.355281650386831,3.48356658627189));
#15694=CARTESIAN_POINT('Ctrl Pts',(7.29235327957763,0.166116376105148,3.42857518785077));
#15695=CARTESIAN_POINT('Ctrl Pts',(7.27644800089002,-0.023048898176535,
3.37358378942964));
#15696=CARTESIAN_POINT('Ctrl Pts',(7.2605427222024,-0.242233201842457,3.42185503634715));
#15697=CARTESIAN_POINT('Ctrl Pts',(7.24463744351479,-0.390796368104757,
3.5512248149675));
#15698=CARTESIAN_POINT('Ctrl Pts',(7.22873216482718,-0.539359534367058,
3.68059459358785));
#15699=CARTESIAN_POINT('Ctrl Pts',(7.21282688613957,-0.617301563225728,
3.89106290391106));
#15700=CARTESIAN_POINT('Ctrl Pts',(7.19692160745195,-0.588834786584626,
4.08599160058025));
#15701=CARTESIAN_POINT('Ctrl Pts',(7.18101632876434,-0.560368009943526,
4.28092029724944));
#15702=CARTESIAN_POINT('Ctrl Pts',(7.16511105007672,-0.425492427802657,
4.46030938026461));
#15703=CARTESIAN_POINT('Ctrl Pts',(7.14920577138911,-0.24613717474127,4.54179097474357));
#15704=CARTESIAN_POINT('Ctrl Pts',(7.1424189846786,-0.169606239833077,4.57655919310821));
#15705=CARTESIAN_POINT('Ctrl Pts',(7.13563219796808,-0.0849767524450092,
4.59350108952231));
#15706=CARTESIAN_POINT('Ctrl Pts',(7.12884541125757,-0.000233413975479213,
4.59320261234329));
#15707=CARTESIAN_POINT('Ctrl Pts',(7.02115458874249,0.000491936389841303,
4.5936290357477));
#15708=CARTESIAN_POINT('Ctrl Pts',(7.03204089516887,-0.135195214358064,
4.59257377495492));
#15709=CARTESIAN_POINT('Ctrl Pts',(7.04292720159524,-0.271531381894462,
4.54641716720817));
#15710=CARTESIAN_POINT('Ctrl Pts',(7.05381350802162,-0.376033620593693,
4.46121547122365));
#15711=CARTESIAN_POINT('Ctrl Pts',(7.06971878670923,-0.528715087097646,
4.33673278019746));
#15712=CARTESIAN_POINT('Ctrl Pts',(7.08562406539685,-0.613443074300594,
4.1289034935015));
#15713=CARTESIAN_POINT('Ctrl Pts',(7.10152934408446,-0.591314251018945,
3.93315398851514));
#15714=CARTESIAN_POINT('Ctrl Pts',(7.11743462277207,-0.569185427737295,
3.73740448352876));
#15715=CARTESIAN_POINT('Ctrl Pts',(7.13333990145968,-0.440199793971044,
3.55373476025198));
#15716=CARTESIAN_POINT('Ctrl Pts',(7.14924518014729,-0.263582002606135,
3.46647820559892));
#15717=CARTESIAN_POINT('Ctrl Pts',(7.16515045883491,-0.0869642112412332,
3.37922165094586));
#15718=CARTESIAN_POINT('Ctrl Pts',(7.18105573752253,0.137285737722324,3.38837826491652));
#15719=CARTESIAN_POINT('Ctrl Pts',(7.19696101621014,0.306201705590428,3.48974370695041));
#15720=CARTESIAN_POINT('Ctrl Pts',(7.21286629489775,0.47511767345854,3.59110914898431));
#15721=CARTESIAN_POINT('Ctrl Pts',(7.22877157358536,0.588699660231196,3.78468341908144));
#15722=CARTESIAN_POINT('Ctrl Pts',(7.24467685227297,0.594795648982816,3.98158540759));
#15723=CARTESIAN_POINT('Ctrl Pts',(7.26058213096058,0.600891637734436,4.17848739609855));
#15724=CARTESIAN_POINT('Ctrl Pts',(7.2764874096482,0.499501628465021,4.37871710301853));
#15725=CARTESIAN_POINT('Ctrl Pts',(7.29239268833581,0.337179610128186,4.49033751492072));
#15726=CARTESIAN_POINT('Ctrl Pts',(7.30197998847137,0.239335998647354,4.5576194790522));
#15727=CARTESIAN_POINT('Ctrl Pts',(7.31156728860693,0.119353510611835,4.59270637405629));
#15728=CARTESIAN_POINT('Ctrl Pts',(7.32115458874249,-0.000317338366111653,
4.59328419319629));
#15729=CARTESIAN_POINT('Origin',(4.,0.,4.));
#15730=CARTESIAN_POINT('',(7.72884541125757,0.000455182276646732,4.59460030787683));
#15731=CARTESIAN_POINT('',(7.62115458874249,-0.000367422317862595,4.59479267874092));
#15732=CARTESIAN_POINT('',(4.,-7.27562663373442E-17,4.5941));
#15733=CARTESIAN_POINT('Ctrl Pts',(7.72884541125757,0.000455182276646732,
4.59460030787683));
#15734=CARTESIAN_POINT('Ctrl Pts',(7.72649554221944,0.0296217258780686,
4.59484761241511));
#15735=CARTESIAN_POINT('Ctrl Pts',(7.72414567318131,0.0587549042441869,
4.59288776399295));
#15736=CARTESIAN_POINT('Ctrl Pts',(7.72179580414318,0.0875427725731367,
4.58860617484604));
#15737=CARTESIAN_POINT('Ctrl Pts',(7.70589052545556,0.282395788279217,4.55962589232715));
#15738=CARTESIAN_POINT('Ctrl Pts',(7.68998524676794,0.461428877889185,4.42427810603975));
#15739=CARTESIAN_POINT('Ctrl Pts',(7.67407996808033,0.542437620895056,4.24470879335187));
#15740=CARTESIAN_POINT('Ctrl Pts',(7.65817468939272,0.623446363900926,4.065139480664));
#15741=CARTESIAN_POINT('Ctrl Pts',(7.64226941070511,0.606430760302702,3.84134864157567));
#15742=CARTESIAN_POINT('Ctrl Pts',(7.6263641320175,0.499203655448083,3.67609156159133));
#15743=CARTESIAN_POINT('Ctrl Pts',(7.61045885332988,0.391976550593464,3.51083448160699));
#15744=CARTESIAN_POINT('Ctrl Pts',(7.59455357464227,0.19453794448245,3.40411116072664));
#15745=CARTESIAN_POINT('Ctrl Pts',(7.57864829595466,-0.00245670798462758,
3.40492443279829));
#15746=CARTESIAN_POINT('Ctrl Pts',(7.56274301726704,-0.199451360451705,
3.40573770486994));
#15747=CARTESIAN_POINT('Ctrl Pts',(7.54683773857943,-0.396002059274846,
3.5140875698936));
#15748=CARTESIAN_POINT('Ctrl Pts',(7.53093245989182,-0.50186103876401,3.68022435377194));
#15749=CARTESIAN_POINT('Ctrl Pts',(7.51502718120421,-0.607720018253171,
3.84636113765028));
#15750=CARTESIAN_POINT('Ctrl Pts',(7.4991219025166,-0.622887278408357,4.07028484038331));
#15751=CARTESIAN_POINT('Ctrl Pts',(7.48321662382898,-0.540398655351294,
4.24917917107494));
#15752=CARTESIAN_POINT('Ctrl Pts',(7.46731134514137,-0.45791003229423,4.42807350176658));
#15753=CARTESIAN_POINT('Ctrl Pts',(7.45140606645375,-0.277765526024924,
4.56193846041682));
#15754=CARTESIAN_POINT('Ctrl Pts',(7.43550078776614,-0.0826798719492015,
4.58930892143267));
#15755=CARTESIAN_POINT('Ctrl Pts',(7.43328232892995,-0.0554694406452989,
4.59312653709876));
#15756=CARTESIAN_POINT('Ctrl Pts',(7.43106387009376,-0.0279683367079049,
4.5948723550368));
#15757=CARTESIAN_POINT('Ctrl Pts',(7.42884541125756,-0.000438237927964824,
4.59464495791636));
#15758=CARTESIAN_POINT('Ctrl Pts',(7.32115458874249,-0.000317338366111653,
4.59328419319629));
#15759=CARTESIAN_POINT('Ctrl Pts',(7.32747256729455,-0.0791797758050172,
4.59366497286126));
#15760=CARTESIAN_POINT('Ctrl Pts',(7.3337905458466,-0.157906876560309,4.57905936436794));
#15761=CARTESIAN_POINT('Ctrl Pts',(7.34010852439865,-0.230073660466993,
4.54880513582638));
#15762=CARTESIAN_POINT('Ctrl Pts',(7.35601380308626,-0.411750885321067,
4.47264122794544));
#15763=CARTESIAN_POINT('Ctrl Pts',(7.37191908177388,-0.551851307624962,
4.29730229529918));
#15764=CARTESIAN_POINT('Ctrl Pts',(7.38782436046149,-0.586046744500155,
4.10329655692985));
#15765=CARTESIAN_POINT('Ctrl Pts',(7.4037296391491,-0.620242181375348,3.90929081856053));
#15766=CARTESIAN_POINT('Ctrl Pts',(7.41963491783671,-0.548532632821828,
3.69661827446815));
#15767=CARTESIAN_POINT('Ctrl Pts',(7.43554019652432,-0.403844087697925,
3.56292915991696));
#15768=CARTESIAN_POINT('Ctrl Pts',(7.45144547521194,-0.259155542574025,
3.42924004536577));
#15769=CARTESIAN_POINT('Ctrl Pts',(7.46735075389955,-0.0414880008797467,
3.37453436035576));
#15770=CARTESIAN_POINT('Ctrl Pts',(7.48325603258717,0.149214809903968,3.42393064079835));
#15771=CARTESIAN_POINT('Ctrl Pts',(7.49916131127478,0.339917620687686,3.47332692124094));
#15772=CARTESIAN_POINT('Ctrl Pts',(7.51506658996239,0.50365570056084,3.62682516713614));
#15773=CARTESIAN_POINT('Ctrl Pts',(7.53097186865001,0.56524745100941,3.81394547807041));
#15774=CARTESIAN_POINT('Ctrl Pts',(7.54687714733762,0.626839201457978,4.00106578900469));
#15775=CARTESIAN_POINT('Ctrl Pts',(7.56278242602523,0.58628462248197,4.22180816497804));
#15776=CARTESIAN_POINT('Ctrl Pts',(7.57868770471284,0.462204660718925,4.3748170457164));
#15777=CARTESIAN_POINT('Ctrl Pts',(7.59284333272272,0.351774041004839,4.51099427596058));
#15778=CARTESIAN_POINT('Ctrl Pts',(7.60699896073261,0.175183620117616,4.59352033541115));
#15779=CARTESIAN_POINT('Ctrl Pts',(7.62115458874249,-0.000367422317862596,
4.59479267874092));
#15780=CARTESIAN_POINT('Origin',(4.,0.,4.));
#15781=CARTESIAN_POINT('',(8.02884541125756,0.000208508845897126,4.59318438507865));
#15782=CARTESIAN_POINT('',(7.92115458874249,0.000504499356536197,4.59443266285439));
#15783=CARTESIAN_POINT('',(4.,-7.27562663373442E-17,4.5941));
#15784=CARTESIAN_POINT('Ctrl Pts',(8.02884541125756,0.000208508845897126,
4.59318438507865));
#15785=CARTESIAN_POINT('Ctrl Pts',(8.02192721434511,0.0865993248636432,
4.5934556945658));
#15786=CARTESIAN_POINT('Ctrl Pts',(8.01500901743265,0.17288466952141,4.57582457789876));
#15787=CARTESIAN_POINT('Ctrl Pts',(8.0080908205202,0.250602156771344,4.53974023855861));
#15788=CARTESIAN_POINT('Ctrl Pts',(7.99218554183259,0.42927852421987,4.4567805482338));
#15789=CARTESIAN_POINT('Ctrl Pts',(7.97628026314498,0.562668370741438,4.27628395749428));
#15790=CARTESIAN_POINT('Ctrl Pts',(7.96037498445736,0.589524722071826,4.08112686462655));
#15791=CARTESIAN_POINT('Ctrl Pts',(7.94446970576975,0.616381073402214,3.88596977175883));
#15792=CARTESIAN_POINT('Ctrl Pts',(7.92856442708213,0.536703929541425,3.67615217676291));
#15793=CARTESIAN_POINT('Ctrl Pts',(7.91265914839452,0.387077664089382,3.54801344261061));
#15794=CARTESIAN_POINT('Ctrl Pts',(7.89675386970691,0.237451398637336,3.41987470845831));
#15795=CARTESIAN_POINT('Ctrl Pts',(7.88084859101929,0.0178760115940344,
3.37341483514963));
#15796=CARTESIAN_POINT('Ctrl Pts',(7.86494331233168,-0.170828768780714,
3.42996623095257));
#15797=CARTESIAN_POINT('Ctrl Pts',(7.84903803364407,-0.359533549155462,
3.48651762675552));
#15798=CARTESIAN_POINT('Ctrl Pts',(7.83313275495647,-0.517367722861657,
3.64608029167009));
#15799=CARTESIAN_POINT('Ctrl Pts',(7.81722747626885,-0.571860514742998,
3.83538980050754));
#15800=CARTESIAN_POINT('Ctrl Pts',(7.80132219758124,-0.626353306624339,
4.02469930934499));
#15801=CARTESIAN_POINT('Ctrl Pts',(7.78541691889362,-0.577504716680827,
4.24375566210532));
#15802=CARTESIAN_POINT('Ctrl Pts',(7.769511640206,-0.447743950807975,4.3919774491103));
#15803=CARTESIAN_POINT('Ctrl Pts',(7.75595623055652,-0.337154229471824,
4.51830073342946));
#15804=CARTESIAN_POINT('Ctrl Pts',(7.74240082090705,-0.16779438404434,4.593173711641));
#15805=CARTESIAN_POINT('Ctrl Pts',(7.72884541125757,0.000455182276646732,
4.59460030787683));
#15806=CARTESIAN_POINT('Ctrl Pts',(7.62115458874249,-0.000367422317862596,
4.59479267874092));
#15807=CARTESIAN_POINT('Ctrl Pts',(7.62290423942022,-0.022065717876263,
4.59494994172972));
#15808=CARTESIAN_POINT('Ctrl Pts',(7.62465389009795,-0.043748134618359,
4.59386587358433));
#15809=CARTESIAN_POINT('Ctrl Pts',(7.62640354077568,-0.0652877816099521,
4.59148835294282));
#15810=CARTESIAN_POINT('Ctrl Pts',(7.64230881946329,-0.261094917625702,
4.56987539392751));
#15811=CARTESIAN_POINT('Ctrl Pts',(7.6582140981509,-0.445103845107109,4.44137409039354));
#15812=CARTESIAN_POINT('Ctrl Pts',(7.67411937683852,-0.532825449416136,
4.2649868044631));
#15813=CARTESIAN_POINT('Ctrl Pts',(7.69002465552613,-0.620547053725161,
4.08859951853267));
#15814=CARTESIAN_POINT('Ctrl Pts',(7.70592993421374,-0.611981334861803,
3.86432625020577));
#15815=CARTESIAN_POINT('Ctrl Pts',(7.72183521290136,-0.511061308497056,
3.69514379608856));
#15816=CARTESIAN_POINT('Ctrl Pts',(7.73774049158897,-0.410141282132307,
3.52596134197134));
#15817=CARTESIAN_POINT('Ctrl Pts',(7.75364577027658,-0.216866948266163,
3.4118697020638));
#15818=CARTESIAN_POINT('Ctrl Pts',(7.76955104896419,-0.0199817042712483,
3.40525493058698));
#15819=CARTESIAN_POINT('Ctrl Pts',(7.78545632765181,0.176903539723664,3.39864015911017));
#15820=CARTESIAN_POINT('Ctrl Pts',(7.80136160633942,0.377399693847348,3.49950225606407));
#15821=CARTESIAN_POINT('Ctrl Pts',(7.81726688502703,0.489447406431712,3.66152961365368));
#15822=CARTESIAN_POINT('Ctrl Pts',(7.83317216371464,0.601495119016078,3.82355697124329));
#15823=CARTESIAN_POINT('Ctrl Pts',(7.84907744240226,0.625094390061116,4.04674958946861));
#15824=CARTESIAN_POINT('Ctrl Pts',(7.86498272108987,0.549409432699027,4.22862686054007));
#15825=CARTESIAN_POINT('Ctrl Pts',(7.88088799977748,0.473724475336938,4.41050413161152));
#15826=CARTESIAN_POINT('Ctrl Pts',(7.89679327846509,0.298755289567731,4.55106605552911));
#15827=CARTESIAN_POINT('Ctrl Pts',(7.91269855715271,0.104840323164387,4.58577254351526));
#15828=CARTESIAN_POINT('Ctrl Pts',(7.9155172343493,0.0704753991278659,4.59192310448195));
#15829=CARTESIAN_POINT('Ctrl Pts',(7.91833591154589,0.0355154700816755,
4.59474920414003));
#15830=CARTESIAN_POINT('Ctrl Pts',(7.92115458874249,0.000504499356536197,
4.59443266285439));
#15831=CARTESIAN_POINT('Origin',(4.,0.,4.));
#15832=CARTESIAN_POINT('',(8.32884541125757,-0.000534402448739424,4.5938336238991));
#15833=CARTESIAN_POINT('',(8.2211545887425,0.000116005647334215,4.59313666129657));
#15834=CARTESIAN_POINT('',(4.,-7.27562663373442E-17,4.5941));
#15835=CARTESIAN_POINT('Ctrl Pts',(8.32884541125757,-0.000534402448739424,
4.5938336238991));
#15836=CARTESIAN_POINT('Ctrl Pts',(8.31735888647079,0.142509087977489,4.59259298046846));
#15837=CARTESIAN_POINT('Ctrl Pts',(8.30587236168401,0.286359812054371,4.54070236535691));
#15838=CARTESIAN_POINT('Ctrl Pts',(8.29438583689723,0.393155811111917,4.44670960845581));
#15839=CARTESIAN_POINT('Ctrl Pts',(8.27848055820962,0.541035187969857,4.31655875596735));
#15840=CARTESIAN_POINT('Ctrl Pts',(8.262575279522,0.617867056310918,4.10568264439756));
#15841=CARTESIAN_POINT('Ctrl Pts',(8.24667000083439,0.588373472681163,3.91090666274675));
#15842=CARTESIAN_POINT('Ctrl Pts',(8.23076472214677,0.558879889051408,3.71613068109593));
#15843=CARTESIAN_POINT('Ctrl Pts',(8.21485944345917,0.423060853450833,3.53745482936408));
#15844=CARTESIAN_POINT('Ctrl Pts',(8.19895416477155,0.243278720997716,3.45691949951456));
#15845=CARTESIAN_POINT('Ctrl Pts',(8.18304888608394,0.0634965885445972,
3.37638416966503));
#15846=CARTESIAN_POINT('Ctrl Pts',(8.16714360739632,-0.160248640761069,
3.39398936169784));
#15847=CARTESIAN_POINT('Ctrl Pts',(8.15123832870871,-0.325222623502191,
3.50165151624576));
#15848=CARTESIAN_POINT('Ctrl Pts',(8.1353330500211,-0.490196606243315,3.60931367079368));
#15849=CARTESIAN_POINT('Ctrl Pts',(8.11942777133349,-0.59639934241989,3.80703278785672));
#15850=CARTESIAN_POINT('Ctrl Pts',(8.10352249264588,-0.595067028646789,
4.00402461368555));
#15851=CARTESIAN_POINT('Ctrl Pts',(8.08761721395827,-0.593734714873688,
4.20101643951437));
#15852=CARTESIAN_POINT('Ctrl Pts',(8.07171193527065,-0.484867351150922,
4.39728097410898));
#15853=CARTESIAN_POINT('Ctrl Pts',(8.05580665658303,-0.3184522251018,4.50270184645125));
#15854=CARTESIAN_POINT('Ctrl Pts',(8.04681957480788,-0.224421408301879,
4.56226861162124));
#15855=CARTESIAN_POINT('Ctrl Pts',(8.03783249303272,-0.112017456676448,
4.59283194056482));
#15856=CARTESIAN_POINT('Ctrl Pts',(8.02884541125756,0.000208508845897126,
4.59318438507865));
#15857=CARTESIAN_POINT('Ctrl Pts',(7.92115458874249,0.000504499356536197,
4.59443266285439));
#15858=CARTESIAN_POINT('Ctrl Pts',(7.93424119023351,-0.162045019349314,
4.59296301969496));
#15859=CARTESIAN_POINT('Ctrl Pts',(7.94732779172453,-0.325694779556815,
4.52375140444135));
#15860=CARTESIAN_POINT('Ctrl Pts',(7.96041439321555,-0.436005268305889,
4.40499428651169));
#15861=CARTESIAN_POINT('Ctrl Pts',(7.97631967190316,-0.570075146335334,
4.26065848946726));
#15862=CARTESIAN_POINT('Ctrl Pts',(7.99222495059077,-0.625354155356748,
4.04313584332371));
#15863=CARTESIAN_POINT('Ctrl Pts',(8.00813022927838,-0.576460513088508,
3.85230354456612));
#15864=CARTESIAN_POINT('Ctrl Pts',(8.024035507966,-0.527566870820267,3.66147124580852));
#15865=CARTESIAN_POINT('Ctrl Pts',(8.03994078665361,-0.374500577262366,
3.49732929443689));
#15866=CARTESIAN_POINT('Ctrl Pts',(8.05584606534123,-0.187543198716277,
3.43524473024767));
#15867=CARTESIAN_POINT('Ctrl Pts',(8.07175134402884,-0.000585820170193818,
3.37316016605846));
#15868=CARTESIAN_POINT('Ctrl Pts',(8.08765662271645,0.220262643364076,3.41313298905166));
#15869=CARTESIAN_POINT('Ctrl Pts',(8.10356190140406,0.37359792075985,3.53680937001953));
#15870=CARTESIAN_POINT('Ctrl Pts',(8.11946718009167,0.526933198155627,3.66048575098741));
#15871=CARTESIAN_POINT('Ctrl Pts',(8.13537245877928,0.612755289412907,3.86786568992997));
#15872=CARTESIAN_POINT('Ctrl Pts',(8.1512777374669,0.591658321059451,4.06372909240644));
#15873=CARTESIAN_POINT('Ctrl Pts',(8.16718301615451,0.570561352705995,4.2595924948829));
#15874=CARTESIAN_POINT('Ctrl Pts',(8.18308829484212,0.44254532474181,4.44393936089328));
#15875=CARTESIAN_POINT('Ctrl Pts',(8.19899357352974,0.266389781296621,4.53212540863836));
#15876=CARTESIAN_POINT('Ctrl Pts',(8.20638057860065,0.184576572093718,4.57308230066594));
#15877=CARTESIAN_POINT('Ctrl Pts',(8.21376758367158,0.0923795717789203,
4.59329710918813));
#15878=CARTESIAN_POINT('Ctrl Pts',(8.2211545887425,0.000116005647334215,
4.59313666129657));
#15879=CARTESIAN_POINT('Origin',(4.,0.,4.));
#15880=CARTESIAN_POINT('',(8.62884541125757,3.48566139269993E-5,4.59507810043999));
#15881=CARTESIAN_POINT('',(8.5211545887425,-0.000547905086566465,4.594005652201));
#15882=CARTESIAN_POINT('',(4.,-7.27562663373442E-17,4.5941));
#15883=CARTESIAN_POINT('Ctrl Pts',(8.62884541125757,3.48566139269993E-5,
4.59507810043999));
#15884=CARTESIAN_POINT('Ctrl Pts',(8.62869583728408,0.00188744051982823,
4.59507966949126));
#15885=CARTESIAN_POINT('Ctrl Pts',(8.62854626331059,0.00374001065808006,
4.59507176912216));
#15886=CARTESIAN_POINT('Ctrl Pts',(8.6283966893371,0.00559249142073073,
4.59505435897699));
#15887=CARTESIAN_POINT('Ctrl Pts',(8.61249141064948,0.202580123064263,4.59320301275402));
#15888=CARTESIAN_POINT('Ctrl Pts',(8.59658613196187,0.398557131004382,4.48381890612783));
#15889=CARTESIAN_POINT('Ctrl Pts',(8.58068085327426,0.503539164298441,4.31712659320126));
#15890=CARTESIAN_POINT('Ctrl Pts',(8.56477557458664,0.608521197592498,4.15043428027469));
#15891=CARTESIAN_POINT('Ctrl Pts',(8.54887029589904,0.622508256240502,3.92643376104774));
#15892=CARTESIAN_POINT('Ctrl Pts',(8.53296501721142,0.539078074654942,3.74797659726896));
#15893=CARTESIAN_POINT('Ctrl Pts',(8.51705973852381,0.455647893069379,3.56951943349019));
#15894=CARTESIAN_POINT('Ctrl Pts',(8.50115445983619,0.274800471250253,3.43660562515959));
#15895=CARTESIAN_POINT('Ctrl Pts',(8.48524918114857,0.0795732942734406,
3.41026356994308));
#15896=CARTESIAN_POINT('Ctrl Pts',(8.46934390246096,-0.115653882703369,
3.38392151472657));
#15897=CARTESIAN_POINT('Ctrl Pts',(8.45343862377335,-0.32526081483786,3.46415121262414));
#15898=CARTESIAN_POINT('Ctrl Pts',(8.43753334508574,-0.453004866631874,
3.61411458059983));
#15899=CARTESIAN_POINT('Ctrl Pts',(8.42162806639813,-0.580748918425883,
3.76407794857552));
#15900=CARTESIAN_POINT('Ctrl Pts',(8.40572278771052,-0.626630089879422,
3.98377498662932));
#15901=CARTESIAN_POINT('Ctrl Pts',(8.3898175090229,-0.569581688133314,4.17233010950212));
#15902=CARTESIAN_POINT('Ctrl Pts',(8.37391223033529,-0.512533286387202,
4.36088523237493));
#15903=CARTESIAN_POINT('Ctrl Pts',(8.35800695164768,-0.352555311441432,
4.51829844006673));
#15904=CARTESIAN_POINT('Ctrl Pts',(8.34210167296007,-0.163102881281137,
4.57229224720906));
#15905=CARTESIAN_POINT('Ctrl Pts',(8.33768291905923,-0.110469810133188,
4.58729263485501));
#15906=CARTESIAN_POINT('Ctrl Pts',(8.3332641651584,-0.0555618361628184,
4.59431088730997));
#15907=CARTESIAN_POINT('Ctrl Pts',(8.32884541125757,-0.000534402448739424,
4.5938336238991));
#15908=CARTESIAN_POINT('Ctrl Pts',(8.2211545887425,0.000116005647334215,
4.59313666129657));
#15909=CARTESIAN_POINT('Ctrl Pts',(8.22967286235919,-0.106277085140544,
4.59295164192424));
#15910=CARTESIAN_POINT('Ctrl Pts',(8.23819113597589,-0.212758691085218,
4.56567285125378));
#15911=CARTESIAN_POINT('Ctrl Pts',(8.24670940959258,-0.303508593564514,
4.51186277431583));
#15912=CARTESIAN_POINT('Ctrl Pts',(8.26261468828019,-0.472956366054245,
4.41138886276846));
#15913=CARTESIAN_POINT('Ctrl Pts',(8.2785199669678,-0.587556852107514,4.21841581019395));
#15914=CARTESIAN_POINT('Ctrl Pts',(8.29442524565541,-0.594690356875377,
4.02154867831793));
#15915=CARTESIAN_POINT('Ctrl Pts',(8.31033052434302,-0.60182386164324,3.82468154644191));
#15916=CARTESIAN_POINT('Ctrl Pts',(8.32623580303064,-0.501490385125681,
3.62392033526436));
#15917=CARTESIAN_POINT('Ctrl Pts',(8.34214108171825,-0.339758814980244,
3.51144609945163));
#15918=CARTESIAN_POINT('Ctrl Pts',(8.35804636040587,-0.178027244834812,
3.3989718636389));
#15919=CARTESIAN_POINT('Ctrl Pts',(8.37395163909348,0.0451024189384938,
3.37478460319097));
#15920=CARTESIAN_POINT('Ctrl Pts',(8.38985691778109,0.227178474572579,3.44999008482693));
#15921=CARTESIAN_POINT('Ctrl Pts',(8.4057621964687,0.40925453020667,3.5251955664629));
#15922=CARTESIAN_POINT('Ctrl Pts',(8.42166747515631,0.550276977701535,3.69979379018275));
#15923=CARTESIAN_POINT('Ctrl Pts',(8.43757275384392,0.585494275335268,3.89361663829603));
#15924=CARTESIAN_POINT('Ctrl Pts',(8.45347803253154,0.620711572969,4.0874394864093));
#15925=CARTESIAN_POINT('Ctrl Pts',(8.46938331121915,0.550123720741606,4.30048695891599));
#15926=CARTESIAN_POINT('Ctrl Pts',(8.48528858990677,0.406141674070155,4.4349366697363));
#15927=CARTESIAN_POINT('Ctrl Pts',(8.49724392285201,0.297916389879728,4.53599689564107));
#15928=CARTESIAN_POINT('Ctrl Pts',(8.50919925579725,0.148224117540273,4.59265016978245));
#15929=CARTESIAN_POINT('Ctrl Pts',(8.5211545887425,-0.000547905086566465,
4.594005652201));
#15930=CARTESIAN_POINT('Origin',(4.,0.,4.));
#15931=CARTESIAN_POINT('',(8.92884541125757,0.000516595407308196,4.59372894893997));
#15932=CARTESIAN_POINT('',(8.82115458874249,0.000142235148737217,4.59503945166131));
#15933=CARTESIAN_POINT('',(4.,-7.27562663373442E-17,4.5941));
#15934=CARTESIAN_POINT('Ctrl Pts',(8.92884541125757,0.000516595407308196,
4.59372894893997));
#15935=CARTESIAN_POINT('Ctrl Pts',(8.92412750940976,0.0592956068199462,
4.59421507565108));
#15936=CARTESIAN_POINT('Ctrl Pts',(8.91940960756194,0.117944888069788,4.58619493689145));
#15937=CARTESIAN_POINT('Ctrl Pts',(8.91469170571413,0.17383025386194,4.56912565303288));
#15938=CARTESIAN_POINT('Ctrl Pts',(8.89878642702651,0.362234410233906,4.51158064138869));
#15939=CARTESIAN_POINT('Ctrl Pts',(8.8828811483389,0.519225559109383,4.35118846702123));
#15940=CARTESIAN_POINT('Ctrl Pts',(8.86697586965128,0.572720006672535,4.16159443076672));
#15941=CARTESIAN_POINT('Ctrl Pts',(8.85107059096367,0.626214454235688,3.97200039451221));
#15942=CARTESIAN_POINT('Ctrl Pts',(8.83516531227606,0.576212200486512,3.75320449637065));
#15943=CARTESIAN_POINT('Ctrl Pts',(8.81926003358845,0.445672164925724,3.60566855627755));
#15944=CARTESIAN_POINT('Ctrl Pts',(8.80335475490084,0.315132129364936,3.45813261618446));
#15945=CARTESIAN_POINT('Ctrl Pts',(8.78744947621322,0.104054311992536,3.38185663413984));
#15946=CARTESIAN_POINT('Ctrl Pts',(8.77154419752561,-0.0906432834200916,
3.41186331412789));
#15947=CARTESIAN_POINT('Ctrl Pts',(8.755638918838,-0.285340878832719,3.44186999411594));
#15948=CARTESIAN_POINT('Ctrl Pts',(8.73973364015038,-0.463658252285575,
3.57815933613666));
#15949=CARTESIAN_POINT('Ctrl Pts',(8.72382836146277,-0.543719609875046,
3.75815304026071));
#15950=CARTESIAN_POINT('Ctrl Pts',(8.70792308277515,-0.623780967464517,
3.93814674438476));
#15951=CARTESIAN_POINT('Ctrl Pts',(8.69201780408754,-0.605586309190603,
4.16184481061213));
#15952=CARTESIAN_POINT('Ctrl Pts',(8.67611252539993,-0.497489852380174,
4.32653455081593));
#15953=CARTESIAN_POINT('Ctrl Pts',(8.66035682068581,-0.390409939629295,
4.48967554111606));
#15954=CARTESIAN_POINT('Ctrl Pts',(8.64460111597169,-0.195111159088962,
4.59491282095998));
#15955=CARTESIAN_POINT('Ctrl Pts',(8.62884541125757,3.48566139269993E-5,
4.59507810043999));
#15956=CARTESIAN_POINT('Ctrl Pts',(8.5211545887425,-0.000547905086566465,
4.594005652201));
#15957=CARTESIAN_POINT('Ctrl Pts',(8.52510453448487,-0.0497009834700827,
4.59445349267793));
#15958=CARTESIAN_POINT('Ctrl Pts',(8.52905448022724,-0.0987536084630192,
4.58886509038946));
#15959=CARTESIAN_POINT('Ctrl Pts',(8.53300442596961,-0.146177075786514,
4.57684766499685));
#15960=CARTESIAN_POINT('Ctrl Pts',(8.54890970465722,-0.337137537856201,
4.52845700030318));
#15961=CARTESIAN_POINT('Ctrl Pts',(8.56481498334483,-0.501682220880061,
4.37582372178193));
#15962=CARTESIAN_POINT('Ctrl Pts',(8.58072026203244,-0.564259167724997,
4.18903057354857));
#15963=CARTESIAN_POINT('Ctrl Pts',(8.59662554072005,-0.626836114569933,
4.00223742531521));
#15964=CARTESIAN_POINT('Ctrl Pts',(8.61253081940767,-0.587445325235947,
3.78128440736974));
#15965=CARTESIAN_POINT('Ctrl Pts',(8.62843609809528,-0.464173383698336,
3.62762379780141));
#15966=CARTESIAN_POINT('Ctrl Pts',(8.6443413767829,-0.340901442160722,3.47396318823307));
#15967=CARTESIAN_POINT('Ctrl Pts',(8.66024665547051,-0.133748348419481,
3.38759498704188));
#15968=CARTESIAN_POINT('Ctrl Pts',(8.67615193415812,0.0621699608040676,
3.40817581827756));
#15969=CARTESIAN_POINT('Ctrl Pts',(8.69205721284573,0.25808827002761,3.42875664951325));
#15970=CARTESIAN_POINT('Ctrl Pts',(8.70796249153334,0.44277179473346,3.55628651317581));
#15971=CARTESIAN_POINT('Ctrl Pts',(8.72386777022095,0.531421673692279,3.73220909121499));
#15972=CARTESIAN_POINT('Ctrl Pts',(8.73977304890857,0.620071552651101,3.90813166925417));
#15973=CARTESIAN_POINT('Ctrl Pts',(8.75567832759618,0.612687785862888,4.13244696166997));
#15974=CARTESIAN_POINT('Ctrl Pts',(8.7715836062838,0.512660686655375,4.30215887618246));
#15975=CARTESIAN_POINT('Ctrl Pts',(8.78748888497141,0.412633587447865,4.47187079069495));
#15976=CARTESIAN_POINT('Ctrl Pts',(8.80339416365902,0.21996315582106,4.58697932730413));
#15977=CARTESIAN_POINT('Ctrl Pts',(8.81929944234663,0.0231155027642346,
4.59463151583965));
#15978=CARTESIAN_POINT('Ctrl Pts',(8.81991782447859,0.0154622529370322,
4.59492902566351));
#15979=CARTESIAN_POINT('Ctrl Pts',(8.82053620661054,0.00780268890311657,
4.59506410656044));
#15980=CARTESIAN_POINT('Ctrl Pts',(8.82115458874249,0.000142235148737217,
4.59503945166131));
#15981=CARTESIAN_POINT('Origin',(4.,0.,4.));
#15982=CARTESIAN_POINT('',(9.22884541125756,-0.000264402795292107,4.59322887297718));
#15983=CARTESIAN_POINT('',(9.12115458874249,0.000475196148639644,4.59357609051269));
#15984=CARTESIAN_POINT('',(4.,-7.27562663373442E-17,4.5941));
#15985=CARTESIAN_POINT('Ctrl Pts',(9.22884541125756,-0.000264402795292107,
4.59322887297718));
#15986=CARTESIAN_POINT('Ctrl Pts',(9.21955918153543,0.115675446261185,4.59276508993807));
#15987=CARTESIAN_POINT('Ctrl Pts',(9.21027295181329,0.231857423975292,4.55999255403315));
#15988=CARTESIAN_POINT('Ctrl Pts',(9.20098672209116,0.327844211240712,4.49662776730038));
#15989=CARTESIAN_POINT('Ctrl Pts',(9.18508144340355,0.492248565587605,4.38809775866155));
#15990=CARTESIAN_POINT('Ctrl Pts',(9.16917616471593,0.597407924103304,4.18982173958679));
#15991=CARTESIAN_POINT('Ctrl Pts',(9.15327088602831,0.595037558282966,3.99283966966863));
#15992=CARTESIAN_POINT('Ctrl Pts',(9.1373656073407,0.592667192462628,3.79585759975047));
#15993=CARTESIAN_POINT('Ctrl Pts',(9.12146032865309,0.482767102306254,3.60016947898891));
#15994=CARTESIAN_POINT('Ctrl Pts',(9.10555504996548,0.315798759724268,3.49562701355602));
#15995=CARTESIAN_POINT('Ctrl Pts',(9.08964977127787,0.148830417142278,3.39108454812312));
#15996=CARTESIAN_POINT('Ctrl Pts',(9.07374449259025,-0.0752061778653251,
3.37768773801888));
#15997=CARTESIAN_POINT('Ctrl Pts',(9.05783921390264,-0.253442899077741,
3.46158783167087));
#15998=CARTESIAN_POINT('Ctrl Pts',(9.04193393521502,-0.431679620290152,
3.54548792532286));
#15999=CARTESIAN_POINT('Ctrl Pts',(9.02602865652741,-0.56411646770738,3.72668492273107));
#16000=CARTESIAN_POINT('Ctrl Pts',(9.0101233778398,-0.589944043936388,3.92198082849844));
#16001=CARTESIAN_POINT('Ctrl Pts',(8.99421809915219,-0.615771620165397,
4.11727673426582));
#16002=CARTESIAN_POINT('Ctrl Pts',(8.97831282046457,-0.534989925206181,
4.32667154839236));
#16003=CARTESIAN_POINT('Ctrl Pts',(8.96240754177696,-0.384690495792338,
4.45402003099517));
#16004=CARTESIAN_POINT('Ctrl Pts',(8.95122016493716,-0.278973620993485,
4.54359378149875));
#16005=CARTESIAN_POINT('Ctrl Pts',(8.94003278809737,-0.138863784294423,
4.59257621560968));
#16006=CARTESIAN_POINT('Ctrl Pts',(8.92884541125757,0.000516595407308196,
4.59372894893997));
#16007=CARTESIAN_POINT('Ctrl Pts',(8.82115458874249,0.000142235148737217,
4.59503945166131));
#16008=CARTESIAN_POINT('Ctrl Pts',(8.83644148529816,-0.189230254871984,
4.59442996300828));
#16009=CARTESIAN_POINT('Ctrl Pts',(8.85172838185382,-0.379146468724227,
4.49620311855542));
#16010=CARTESIAN_POINT('Ctrl Pts',(8.86701527840948,-0.487657002993039,
4.34104488491935));
#16011=CARTESIAN_POINT('Ctrl Pts',(8.88292055709709,-0.600556981206626,
4.17961022500168));
#16012=CARTESIAN_POINT('Ctrl Pts',(8.89882583578469,-0.62533206314696,3.95654506470448));
#16013=CARTESIAN_POINT('Ctrl Pts',(8.91473111447231,-0.550606579334316,
3.77427148852754));
#16014=CARTESIAN_POINT('Ctrl Pts',(8.93063639315992,-0.47588109552167,3.5919979123506));
#16015=CARTESIAN_POINT('Ctrl Pts',(8.94654167184753,-0.301655045956043,
3.45051592029392));
#16016=CARTESIAN_POINT('Ctrl Pts',(8.96244695053515,-0.107925661701669,
3.41478805750048));
#16017=CARTESIAN_POINT('Ctrl Pts',(8.97835222922276,0.0858037225526985,
3.37906019470703));
#16018=CARTESIAN_POINT('Ctrl Pts',(8.99425750791037,0.299036441495806,3.4490864611768));
#16019=CARTESIAN_POINT('Ctrl Pts',(9.01016278659798,0.433865051721373,3.5927137579139));
#16020=CARTESIAN_POINT('Ctrl Pts',(9.0260680652856,0.568693661946943,3.736341054651));
#16021=CARTESIAN_POINT('Ctrl Pts',(9.04197334397321,0.625118163454969,3.95356938165542));
#16022=CARTESIAN_POINT('Ctrl Pts',(9.05787862266082,0.577230812276762,4.14465668133936));
#16023=CARTESIAN_POINT('Ctrl Pts',(9.07378390134844,0.529343461098555,4.3357439810233));
#16024=CARTESIAN_POINT('Ctrl Pts',(9.08968918003605,0.377144257234124,4.50069025338676));
#16025=CARTESIAN_POINT('Ctrl Pts',(9.10559445872366,0.190516636080703,4.56375914846174));
#16026=CARTESIAN_POINT('Ctrl Pts',(9.11078116872994,0.129657384941762,4.58432590969837));
#16027=CARTESIAN_POINT('Ctrl Pts',(9.11596787873622,0.0651369761893139,
4.59405891310139));
#16028=CARTESIAN_POINT('Ctrl Pts',(9.12115458874249,0.000475196148639644,
4.59357609051269));
#16029=CARTESIAN_POINT('Origin',(4.,0.,4.));
#16030=CARTESIAN_POINT('',(9.52884541125756,-0.000414715089906426,4.59470005288553));
#16031=CARTESIAN_POINT('',(9.4211545887425,-0.000345133784900094,4.59331940772745));
#16032=CARTESIAN_POINT('',(4.,-7.27562663373442E-17,4.5941));
#16033=CARTESIAN_POINT('Ctrl Pts',(9.52884541125756,-0.000414715089906426,
4.59470005288553));
#16034=CARTESIAN_POINT('Ctrl Pts',(9.5149908536611,0.17147269131647,4.59333531965569));
#16035=CARTESIAN_POINT('Ctrl Pts',(9.50113629606464,0.344448366351018,4.51470554290992));
#16036=CARTESIAN_POINT('Ctrl Pts',(9.48728173846818,0.455032043431697,4.38349290156166));
#16037=CARTESIAN_POINT('Ctrl Pts',(9.47137645978057,0.581984072756561,4.23285845412795));
#16038=CARTESIAN_POINT('Ctrl Pts',(9.45547118109296,0.626706888961734,4.01292269047354));
#16039=CARTESIAN_POINT('Ctrl Pts',(9.43956590240535,0.56866566691212,3.82467080855373));
#16040=CARTESIAN_POINT('Ctrl Pts',(9.42366062371773,0.510624444862503,3.63641892663391));
#16041=CARTESIAN_POINT('Ctrl Pts',(9.40775534503012,0.349819184558098,3.47985092644869));
#16042=CARTESIAN_POINT('Ctrl Pts',(9.39185006634251,0.160084858421151,3.42685620983728));
#16043=CARTESIAN_POINT('Ctrl Pts',(9.37594478765489,-0.0296494677157886,
3.37386149322587));
#16044=CARTESIAN_POINT('Ctrl Pts',(9.36003950896728,-0.248312859685263,
3.42444006018826));
#16045=CARTESIAN_POINT('Ctrl Pts',(9.34413423027966,-0.395504338780113,
3.55536837257802));
#16046=CARTESIAN_POINT('Ctrl Pts',(9.32822895159205,-0.542695817874971,
3.6862966849678));
#16047=CARTESIAN_POINT('Ctrl Pts',(9.31232367290444,-0.618415384095196,
3.89757474278496));
#16048=CARTESIAN_POINT('Ctrl Pts',(9.29641839421683,-0.587895816063128,
4.09219260031737));
#16049=CARTESIAN_POINT('Ctrl Pts',(9.28051311552922,-0.55737624803106,4.28681045784976));
#16050=CARTESIAN_POINT('Ctrl Pts',(9.26460783684159,-0.42061754574671,4.4647681150974));
#16051=CARTESIAN_POINT('Ctrl Pts',(9.24870255815398,-0.240413519515492,
4.54435494461976));
#16052=CARTESIAN_POINT('Ctrl Pts',(9.24208350918851,-0.165420852186184,
4.57747534017911));
#16053=CARTESIAN_POINT('Ctrl Pts',(9.23546446022304,-0.0829041350566004,
4.59355944875842));
#16054=CARTESIAN_POINT('Ctrl Pts',(9.22884541125756,-0.000264402795292107,
4.59322887297718));
#16055=CARTESIAN_POINT('Ctrl Pts',(9.12115458874249,0.000475196148639644,
4.59357609051269));
#16056=CARTESIAN_POINT('Ctrl Pts',(9.13187315742383,-0.133151270259641,
4.59257831599443));
#16057=CARTESIAN_POINT('Ctrl Pts',(9.14259172610516,-0.267381477949042,
4.54795275857003));
#16058=CARTESIAN_POINT('Ctrl Pts',(9.1533102947865,-0.371151898503526,4.46515291500219));
#16059=CARTESIAN_POINT('Ctrl Pts',(9.16921557347411,-0.525136773491911,
4.34228626868117));
#16060=CARTESIAN_POINT('Ctrl Pts',(9.18512085216173,-0.612050485026272,
4.13536145825263));
#16061=CARTESIAN_POINT('Ctrl Pts',(9.20102613084934,-0.591985933785934,
3.93938960239856));
#16062=CARTESIAN_POINT('Ctrl Pts',(9.21693140953695,-0.571921382545595,
3.74341774654449));
#16063=CARTESIAN_POINT('Ctrl Pts',(9.23283668822456,-0.444878568530549,
3.55839884526489));
#16064=CARTESIAN_POINT('Ctrl Pts',(9.24874196691217,-0.269190177198291,
3.46928575052316));
#16065=CARTESIAN_POINT('Ctrl Pts',(9.26464724559978,-0.0935017858660342,
3.38017265578144));
#16066=CARTESIAN_POINT('Ctrl Pts',(9.28055252428739,0.130832182783434,3.38696536757758));
#16067=CARTESIAN_POINT('Ctrl Pts',(9.29645780297501,0.300807061133818,3.48654496003073));
#16068=CARTESIAN_POINT('Ctrl Pts',(9.31236308166262,0.470781939484206,3.58612455248389));
#16069=CARTESIAN_POINT('Ctrl Pts',(9.32826836035024,0.586397727535503,3.77849102559406));
#16070=CARTESIAN_POINT('Ctrl Pts',(9.34417363903785,0.594568546715174,3.97531783326339));
#16071=CARTESIAN_POINT('Ctrl Pts',(9.36007891772546,0.602739365894845,4.17214464093271));
#16072=CARTESIAN_POINT('Ctrl Pts',(9.37598419641307,0.503465216202894,4.37343178316119));
#16073=CARTESIAN_POINT('Ctrl Pts',(9.39188947510069,0.342328587234952,4.48675671999422));
#16074=CARTESIAN_POINT('Ctrl Pts',(9.40164451298129,0.243500144778355,4.55626125828842));
#16075=CARTESIAN_POINT('Ctrl Pts',(9.41139955086189,0.121401365174849,4.59267772446372));
#16076=CARTESIAN_POINT('Ctrl Pts',(9.4211545887425,-0.000345133784900094,
4.59331940772745));
#16077=CARTESIAN_POINT('Origin',(4.,0.,4.));
#16078=CARTESIAN_POINT('',(9.82884541125756,0.000474857175501747,4.59454166667424));
#16079=CARTESIAN_POINT('',(9.7211545887425,-0.000338423355870402,4.59484023865297));
#16080=CARTESIAN_POINT('',(4.,-7.27562663373442E-17,4.5941));
#16081=CARTESIAN_POINT('Ctrl Pts',(9.82884541125756,0.000474857175501747,
4.59454166667424));
#16082=CARTESIAN_POINT('Ctrl Pts',(9.82632780447438,0.0317313679687054,
4.59481419231428));
#16083=CARTESIAN_POINT('Ctrl Pts',(9.82381019769121,0.0629485386443197,
4.59256288124703));
#16084=CARTESIAN_POINT('Ctrl Pts',(9.82129259090804,0.093741277189286,4.58765086492638));
#16085=CARTESIAN_POINT('Ctrl Pts',(9.80538731222043,0.288278045752977,4.55661862072519));
#16086=CARTESIAN_POINT('Ctrl Pts',(9.78948203353282,0.465874751366426,4.41939150759219));
#16087=CARTESIAN_POINT('Ctrl Pts',(9.77357675484521,0.54498650030893,4.23897841027765));
#16088=CARTESIAN_POINT('Ctrl Pts',(9.7576714761576,0.624098249251433,4.05856531296313));
#16089=CARTESIAN_POINT('Ctrl Pts',(9.74176619746998,0.604725041522997,3.83496623146707));
#16090=CARTESIAN_POINT('Ctrl Pts',(9.72586091878237,0.495762234499694,3.67084840431546));
#16091=CARTESIAN_POINT('Ctrl Pts',(9.70995564009475,0.386799427476386,3.50673057716384));
#16092=CARTESIAN_POINT('Ctrl Pts',(9.69405036140714,0.188247021158209,3.40209400435668));
#16093=CARTESIAN_POINT('Ctrl Pts',(9.67814508271953,-0.00872811953311764,
3.40498337331868));
#16094=CARTESIAN_POINT('Ctrl Pts',(9.66223980403192,-0.205703260224436,
3.40787274228067));
#16095=CARTESIAN_POINT('Ctrl Pts',(9.6463345253443,-0.4011011352889,3.51828805301183));
#16096=CARTESIAN_POINT('Ctrl Pts',(9.63042924665669,-0.505203307099277,
3.68553126611098));
#16097=CARTESIAN_POINT('Ctrl Pts',(9.61452396796908,-0.609305478909656,
3.85277447921013));
#16098=CARTESIAN_POINT('Ctrl Pts',(9.59861868928147,-0.622111947465945,
4.07684559467727));
#16099=CARTESIAN_POINT('Ctrl Pts',(9.58271341059386,-0.537742524204099,
4.25486063595701));
#16100=CARTESIAN_POINT('Ctrl Pts',(9.56680813190624,-0.453373100942255,
4.43287567723675));
#16101=CARTESIAN_POINT('Ctrl Pts',(9.55090285321863,-0.271827785862281,
4.5648346443291));
#16102=CARTESIAN_POINT('Ctrl Pts',(9.53499757453102,-0.0764645071000137,
4.59014756226876));
#16103=CARTESIAN_POINT('Ctrl Pts',(9.53294685343987,-0.0512756623106346,
4.5934112419387));
#16104=CARTESIAN_POINT('Ctrl Pts',(9.53089613234871,-0.025857110284879,
4.59490205769144));
#16105=CARTESIAN_POINT('Ctrl Pts',(9.52884541125756,-0.000414715089906426,
4.59470005288553));
#16106=CARTESIAN_POINT('Ctrl Pts',(9.4211545887425,-0.000345133784900094,
4.59331940772745));
#16107=CARTESIAN_POINT('Ctrl Pts',(9.42730482954951,-0.0771024252662454,
4.59372396859559));
#16108=CARTESIAN_POINT('Ctrl Pts',(9.43345507035652,-0.153719688677923,
4.57990840728947));
#16109=CARTESIAN_POINT('Ctrl Pts',(9.43960531116353,-0.224276981305518,
4.55119942103951));
#16110=CARTESIAN_POINT('Ctrl Pts',(9.45551058985114,-0.406746812634079,
4.47695445381419));
#16111=CARTESIAN_POINT('Ctrl Pts',(9.47141586853875,-0.548687367047265,
4.30310178792596));
#16112=CARTESIAN_POINT('Ctrl Pts',(9.48732114722636,-0.58492554696818,4.10946721245096));
#16113=CARTESIAN_POINT('Ctrl Pts',(9.50322642591398,-0.621163726889096,
3.91583263697596));
#16114=CARTESIAN_POINT('Ctrl Pts',(9.5191317046016,-0.55169953231774,3.70241615191419));
#16115=CARTESIAN_POINT('Ctrl Pts',(9.53503698328921,-0.408427982613559,
3.56720957829912));
#16116=CARTESIAN_POINT('Ctrl Pts',(9.55094226197682,-0.265156432909381,
3.43200300468405));
#16117=CARTESIAN_POINT('Ctrl Pts',(9.56684754066442,-0.0480775280723801,
3.37500634251568));
#16118=CARTESIAN_POINT('Ctrl Pts',(9.58275281935204,0.14313528264739,3.42239004773181));
#16119=CARTESIAN_POINT('Ctrl Pts',(9.59865809803965,0.334348093367161,3.46977375294793));
#16120=CARTESIAN_POINT('Ctrl Pts',(9.61456337672728,0.499694809969701,3.62153782554855));
#16121=CARTESIAN_POINT('Ctrl Pts',(9.63046865541489,0.563255215433827,3.80799862400389));
#16122=CARTESIAN_POINT('Ctrl Pts',(9.6463739341025,0.626815620897955,3.99445942245922));
#16123=CARTESIAN_POINT('Ctrl Pts',(9.6622792127901,0.588589715223662,4.21561694676927));
#16124=CARTESIAN_POINT('Ctrl Pts',(9.67818449147771,0.466129217091882,4.36992501817411));
#16125=CARTESIAN_POINT('Ctrl Pts',(9.69250785723264,0.355848439261942,4.50888586187125));
#16126=CARTESIAN_POINT('Ctrl Pts',(9.70683122298757,0.177255492135987,4.59363345408847));
#16127=CARTESIAN_POINT('Ctrl Pts',(9.7211545887425,-0.000338423355870402,
4.59484023865297));
#16128=CARTESIAN_POINT('Origin',(4.,0.,4.));
#16129=CARTESIAN_POINT('',(10.1288454112576,0.000175993811045716,4.59316417414361));
#16130=CARTESIAN_POINT('',(10.0211545887425,0.000517772199431355,4.59437035498519));
#16131=CARTESIAN_POINT('',(4.,-7.27562663373442E-17,4.5941));
#16132=CARTESIAN_POINT('Ctrl Pts',(10.1288454112576,0.000175993811045716,
4.59316417414361));
#16133=CARTESIAN_POINT('Ctrl Pts',(10.1217594766001,0.0886689559287146,
4.59339827721605));
#16134=CARTESIAN_POINT('Ctrl Pts',(10.1146735419426,0.177068724884878,4.57486525982572));
#16135=CARTESIAN_POINT('Ctrl Pts',(10.1075876072851,0.256276603526552,4.53706914692868));
#16136=CARTESIAN_POINT('Ctrl Pts',(10.0916823285975,0.434068729046268,4.45223097977176));
#16137=CARTESIAN_POINT('Ctrl Pts',(10.0757770499098,0.565548899719798,4.27033860735548));
#16138=CARTESIAN_POINT('Ctrl Pts',(10.0598717712222,0.590346983641159,4.0749093118617));
#16139=CARTESIAN_POINT('Ctrl Pts',(10.0439664925346,0.61514506756252,3.87948001636793));
#16140=CARTESIAN_POINT('Ctrl Pts',(10.028061213847,0.533261064731712,3.67051379779667));
#16141=CARTESIAN_POINT('Ctrl Pts',(10.0121559351594,0.382292645022166,3.5439591030842));
#16142=CARTESIAN_POINT('Ctrl Pts',(9.99625065647179,0.231324225312614,3.41740440837173));
#16143=CARTESIAN_POINT('Ctrl Pts',(9.98034537778417,0.011271388724311,3.37326123751805));
#16144=CARTESIAN_POINT('Ctrl Pts',(9.96444009909655,-0.17682691184915,3.43179826703564));
#16145=CARTESIAN_POINT('Ctrl Pts',(9.94853482040894,-0.364925212422603,
3.49033529655323));
#16146=CARTESIAN_POINT('Ctrl Pts',(9.93262954172133,-0.521068976981223,
3.65155252644206));
#16147=CARTESIAN_POINT('Ctrl Pts',(9.91672426303372,-0.573563594737602,
3.84142582527571));
#16148=CARTESIAN_POINT('Ctrl Pts',(9.90081898434611,-0.626058212493981,
4.03129912410937));
#16149=CARTESIAN_POINT('Ctrl Pts',(9.8849137056585,-0.574903683448118,4.24982849188785));
#16150=CARTESIAN_POINT('Ctrl Pts',(9.86900842697089,-0.443588003168223,
4.39667448814241));
#16151=CARTESIAN_POINT('Ctrl Pts',(9.85562075506645,-0.333057953489513,
4.52027659892262));
#16152=CARTESIAN_POINT('Ctrl Pts',(9.842233083162,-0.165735336637852,4.59309247934331));
#16153=CARTESIAN_POINT('Ctrl Pts',(9.82884541125756,0.000474857175501747,
4.59454166667424));
#16154=CARTESIAN_POINT('Ctrl Pts',(9.7211545887425,-0.000338423355870402,
4.59484023865297));
#16155=CARTESIAN_POINT('Ctrl Pts',(9.72273650167518,-0.0199523965301825,
4.59497351934566));
#16156=CARTESIAN_POINT('Ctrl Pts',(9.72431841460787,-0.0395541838993478,
4.59408780127083));
#16157=CARTESIAN_POINT('Ctrl Pts',(9.72590032754056,-0.0590504136254521,
4.592143576127));
#16158=CARTESIAN_POINT('Ctrl Pts',(9.74180560622817,-0.255074455621757,
4.57259544417541));
#16159=CARTESIAN_POINT('Ctrl Pts',(9.75771088491579,-0.4404274490251,4.4460405617726));
#16160=CARTESIAN_POINT('Ctrl Pts',(9.7736161636034,-0.530003140903138,4.2705875768224));
#16161=CARTESIAN_POINT('Ctrl Pts',(9.78952144229101,-0.619578832781174,
4.0951345918722));
#16162=CARTESIAN_POINT('Ctrl Pts',(9.80542672097862,-0.61337722313391,3.87078350437461));
#16163=CARTESIAN_POINT('Ctrl Pts',(9.82133199966623,-0.514245828742901,
3.70054684219675));
#16164=CARTESIAN_POINT('Ctrl Pts',(9.83723727835384,-0.41511443435189,3.53031018001889));
#16165=CARTESIAN_POINT('Ctrl Pts',(9.85314255704146,-0.223053255217129,
3.41418794316076));
#16166=CARTESIAN_POINT('Ctrl Pts',(9.86904783572907,-0.0262486593588972,
3.40549855006092));
#16167=CARTESIAN_POINT('Ctrl Pts',(9.88495311441669,0.170555936499329,3.39680915696108));
#16168=CARTESIAN_POINT('Ctrl Pts',(9.9008583931043,0.372103949081026,3.49555260761951));
#16169=CARTESIAN_POINT('Ctrl Pts',(9.91676367179191,0.485853057801912,3.65639008698476));
#16170=CARTESIAN_POINT('Ctrl Pts',(9.93266895047952,0.5996021665228,3.81722756635002));
#16171=CARTESIAN_POINT('Ctrl Pts',(9.94857422916713,0.625552371382872,4.04015907442209));
#16172=CARTESIAN_POINT('Ctrl Pts',(9.96447950785475,0.551788436173011,4.22282389414861));
#16173=CARTESIAN_POINT('Ctrl Pts',(9.98038478654236,0.478024500963153,4.40548871387512));
#16174=CARTESIAN_POINT('Ctrl Pts',(9.99629006522997,0.304546425683368,4.54788684525607));
#16175=CARTESIAN_POINT('Ctrl Pts',(10.0121953439176,0.111008003250015,4.58463509072946));
#16176=CARTESIAN_POINT('Ctrl Pts',(10.0151817588592,0.0746687445744621,
4.59153503329043));
#16177=CARTESIAN_POINT('Ctrl Pts',(10.0181681738009,0.0376222632219309,
4.59471031472953));
#16178=CARTESIAN_POINT('Ctrl Pts',(10.0211545887425,0.000517772199431355,
4.59437035498519));
#16179=CARTESIAN_POINT('Origin',(4.,0.,4.));
#16180=CARTESIAN_POINT('',(10.4288454112576,-0.000541293539476018,4.59389423388278));
#16181=CARTESIAN_POINT('',(10.3211545887425,8.19078234495683E-5,4.59312629593825));
#16182=CARTESIAN_POINT('',(4.,-7.27562663373442E-17,4.5941));
#16183=CARTESIAN_POINT('Ctrl Pts',(10.4288454112576,-0.000541293539476018,
4.59389423388278));
#16184=CARTESIAN_POINT('Ctrl Pts',(10.4171911487257,0.144553461780974,4.59260897165526));
#16185=CARTESIAN_POINT('Ctrl Pts',(10.4055368861939,0.290497422953868,4.53904330389552));
#16186=CARTESIAN_POINT('Ctrl Pts',(10.3938826236621,0.397841883685798,4.4425412994096));
#16187=CARTESIAN_POINT('Ctrl Pts',(10.3779773449745,0.544341377656434,4.31083916286766));
#16188=CARTESIAN_POINT('Ctrl Pts',(10.3620720662869,0.618946539098701,4.09916502578488));
#16189=CARTESIAN_POINT('Ctrl Pts',(10.3461667875993,0.587401834162399,3.90471069671543));
#16190=CARTESIAN_POINT('Ctrl Pts',(10.3302615089117,0.555857129226098,3.710256367646));
#16191=CARTESIAN_POINT('Ctrl Pts',(10.314356230224,0.418162557911234,3.5330218465899));
#16192=CARTESIAN_POINT('Ctrl Pts',(10.2984509515364,0.237541641988682,3.45438572744188));
#16193=CARTESIAN_POINT('Ctrl Pts',(10.2825456728488,0.0569207260661262,
3.37574960829385));
#16194=CARTESIAN_POINT('Ctrl Pts',(10.2666403941612,-0.16662653446412,3.3957118910539));
#16195=CARTESIAN_POINT('Ctrl Pts',(10.2507351154736,-0.330456695071223,
3.50510674001315));
#16196=CARTESIAN_POINT('Ctrl Pts',(10.234829836786,-0.494286855678321,3.61450158897239));
#16197=CARTESIAN_POINT('Ctrl Pts',(10.2189245580984,-0.59839991636228,3.81332900413083));
#16198=CARTESIAN_POINT('Ctrl Pts',(10.2030192794108,-0.594991564317383,
4.01029584814195));
#16199=CARTESIAN_POINT('Ctrl Pts',(10.1871140007231,-0.591583212272486,
4.20726269215308));
#16200=CARTESIAN_POINT('Ctrl Pts',(10.1712087220355,-0.480653447498727,
4.40236896501689));
#16201=CARTESIAN_POINT('Ctrl Pts',(10.1553034433479,-0.313136524928893,
4.50603012050002));
#16202=CARTESIAN_POINT('Ctrl Pts',(10.1464840993178,-0.220249792163878,
4.56350936438632));
#16203=CARTESIAN_POINT('Ctrl Pts',(10.1376647552877,-0.109964716607974,
4.59287280319057));
#16204=CARTESIAN_POINT('Ctrl Pts',(10.1288454112576,0.000175993811045716,
4.59316417414361));
#16205=CARTESIAN_POINT('Ctrl Pts',(10.0211545887425,0.000517772199431355,
4.59437035498519));
#16206=CARTESIAN_POINT('Ctrl Pts',(10.0340734524885,-0.159991692577292,
4.59289973094197));
#16207=CARTESIAN_POINT('Ctrl Pts',(10.0469923162344,-0.321586704601994,
4.52564765365589));
#16208=CARTESIAN_POINT('Ctrl Pts',(10.0599111799804,-0.431712787135162,
4.40956688772629));
#16209=CARTESIAN_POINT('Ctrl Pts',(10.075816458668,-0.567296385500051,4.2666520796839));
#16210=CARTESIAN_POINT('Ctrl Pts',(10.0917217373556,-0.624864812642908,
4.04972410403331));
#16211=CARTESIAN_POINT('Ctrl Pts',(10.1076270160433,-0.577985082339038,
3.85838710972745));
#16212=CARTESIAN_POINT('Ctrl Pts',(10.1235322947309,-0.531105352035168,
3.6670501154216));
#16213=CARTESIAN_POINT('Ctrl Pts',(10.1394375734185,-0.379777464284567,
3.50130410246047));
#16214=CARTESIAN_POINT('Ctrl Pts',(10.1553428521061,-0.193484782987353,
3.43725262786029));
#16215=CARTESIAN_POINT('Ctrl Pts',(10.1712481307937,-0.00719210169012799,
3.37320115326011));
#16216=CARTESIAN_POINT('Ctrl Pts',(10.1871534094813,0.214065373153706,3.41084421702088));
#16217=CARTESIAN_POINT('Ctrl Pts',(10.2030586881689,0.368695569727689,3.53289771681035));
#16218=CARTESIAN_POINT('Ctrl Pts',(10.2189639668565,0.523325766301663,3.65495121659981));
#16219=CARTESIAN_POINT('Ctrl Pts',(10.2348692455442,0.611328684605784,3.86141515241798));
#16220=CARTESIAN_POINT('Ctrl Pts',(10.2507745242318,0.592297107651237,4.05749001970593));
#16221=CARTESIAN_POINT('Ctrl Pts',(10.2666798029194,0.573265530696689,4.25356488699388));
#16222=CARTESIAN_POINT('Ctrl Pts',(10.282585081607,0.447199458483466,4.43925068575162));
#16223=CARTESIAN_POINT('Ctrl Pts',(10.2984903602946,0.271983097956201,4.5292883529079));
#16224=CARTESIAN_POINT('Ctrl Pts',(10.3060451031106,0.188758241169316,4.57205474716445));
#16225=CARTESIAN_POINT('Ctrl Pts',(10.3135998459265,0.0944446272328244,
4.59324204311815));
#16226=CARTESIAN_POINT('Ctrl Pts',(10.3211545887425,8.19078234495684E-5,
4.59312629593825));
#16227=CARTESIAN_POINT('Origin',(4.,0.,4.));
#16228=CARTESIAN_POINT('',(10.7288454112576,7.37317986114466E-5,4.59506942345298));
#16229=CARTESIAN_POINT('',(10.6211545887425,-0.000548317120500629,4.59406879148573));
#16230=CARTESIAN_POINT('',(4.,-7.27562663373442E-17,4.5941));
#16231=CARTESIAN_POINT('Ctrl Pts',(10.7288454112576,7.37317986114466E-5,
4.59506942345298));
#16232=CARTESIAN_POINT('Ctrl Pts',(10.728528099539,0.00400402563557926,
4.59507627971693));
#16233=CARTESIAN_POINT('Ctrl Pts',(10.7282107878205,0.00793419209028873,
4.59504072157671));
#16234=CARTESIAN_POINT('Ctrl Pts',(10.727893476102,0.0118635052742893,4.59496237136513));
#16235=CARTESIAN_POINT('Ctrl Pts',(10.7119881974144,0.208820685209451,4.59103505989901));
#16236=CARTESIAN_POINT('Ctrl Pts',(10.6960829187267,0.403634001393415,4.47959161118634));
#16237=CARTESIAN_POINT('Ctrl Pts',(10.6801776400391,0.506853420906232,4.31180214209248));
#16238=CARTESIAN_POINT('Ctrl Pts',(10.6642723613515,0.610072840419052,4.14401267299861));
#16239=CARTESIAN_POINT('Ctrl Pts',(10.6483670826639,0.621698363260717,3.91987718352354));
#16240=CARTESIAN_POINT('Ctrl Pts',(10.6324618039763,0.536392041177647,3.74230920804366));
#16241=CARTESIAN_POINT('Ctrl Pts',(10.6165565252887,0.451085719094577,3.56474123256377));
#16242=CARTESIAN_POINT('Ctrl Pts',(10.6006512466011,0.26884755208677,3.43374077107907));
#16243=CARTESIAN_POINT('Ctrl Pts',(10.5847459679135,0.0733535965831807,
3.40945769333085));
#16244=CARTESIAN_POINT('Ctrl Pts',(10.5688406892258,-0.122140358920403,
3.38517461558263));
#16245=CARTESIAN_POINT('Ctrl Pts',(10.5529354105382,-0.33089010291977,3.46760892157089));
#16246=CARTESIAN_POINT('Ctrl Pts',(10.5370301318506,-0.457046584443773,
3.61891026549369));
#16247=CARTESIAN_POINT('Ctrl Pts',(10.521124853163,-0.583203065967777,3.7702116094165));
#16248=CARTESIAN_POINT('Ctrl Pts',(10.5052195744754,-0.626766285016417,
3.99037999127385));
#16249=CARTESIAN_POINT('Ctrl Pts',(10.4893142957878,-0.567733854410369,
4.17832340467295));
#16250=CARTESIAN_POINT('Ctrl Pts',(10.4734090171002,-0.508701423804317,
4.36626681807206));
#16251=CARTESIAN_POINT('Ctrl Pts',(10.4575037384126,-0.347073343543565,
4.52198526301292));
#16252=CARTESIAN_POINT('Ctrl Pts',(10.4415984597249,-0.157062390163684,
4.57397941748279));
#16253=CARTESIAN_POINT('Ctrl Pts',(10.4373474435692,-0.106278015462724,
4.58787593542499));
#16254=CARTESIAN_POINT('Ctrl Pts',(10.4330964274134,-0.0534661480554494,
4.59436304694399));
#16255=CARTESIAN_POINT('Ctrl Pts',(10.4288454112576,-0.000541293539476018,
4.59389423388278));
#16256=CARTESIAN_POINT('Ctrl Pts',(10.3211545887425,8.19078234495684E-5,
4.59312629593825));
#16257=CARTESIAN_POINT('Ctrl Pts',(10.3295051246142,-0.104220686264852,
4.59299835631127));
#16258=CARTESIAN_POINT('Ctrl Pts',(10.3378556604858,-0.208583275928277,
4.56684300569277));
#16259=CARTESIAN_POINT('Ctrl Pts',(10.3462061963575,-0.298097175589899,
4.5150330474864));
#16260=CARTESIAN_POINT('Ctrl Pts',(10.3621114750451,-0.468594439767441,
4.41635053935381));
#16261=CARTESIAN_POINT('Ctrl Pts',(10.3780167537327,-0.585222319281217,
4.22459598753381));
#16262=CARTESIAN_POINT('Ctrl Pts',(10.3939220324203,-0.594430225977177,
4.02781496975607));
#16263=CARTESIAN_POINT('Ctrl Pts',(10.4098273111079,-0.603638132673137,
3.83103395197833));
#16264=CARTESIAN_POINT('Ctrl Pts',(10.4257325897955,-0.505426066551287,
3.62922646824286));
#16265=CARTESIAN_POINT('Ctrl Pts',(10.4416378684831,-0.344888853364916,
3.51505397731042));
#16266=CARTESIAN_POINT('Ctrl Pts',(10.4575431471707,-0.184351640178541,
3.40088148637798));
#16267=CARTESIAN_POINT('Ctrl Pts',(10.4734484258584,0.0385107200723601,
3.37434398824859));
#16268=CARTESIAN_POINT('Ctrl Pts',(10.489353704546,0.221369260089487,3.4476263793543));
#16269=CARTESIAN_POINT('Ctrl Pts',(10.5052589832336,0.40422780010661,3.52090877046001));
#16270=CARTESIAN_POINT('Ctrl Pts',(10.5211642619212,0.54708251988996,3.69401105080081));
#16271=CARTESIAN_POINT('Ctrl Pts',(10.5370695406088,0.584340575799814,3.88745197659776));
#16272=CARTESIAN_POINT('Ctrl Pts',(10.5529748192964,0.621598631709669,4.08089290239472));
#16273=CARTESIAN_POINT('Ctrl Pts',(10.568880097984,0.55326002374602,4.29467247364782));
#16274=CARTESIAN_POINT('Ctrl Pts',(10.5847853766716,0.4107029495177,4.43063215550545));
#16275=CARTESIAN_POINT('Ctrl Pts',(10.5969084473619,0.302045344566967,4.53426120008624));
#16276=CARTESIAN_POINT('Ctrl Pts',(10.6090315180522,0.150270129189204,4.59268036842864));
#16277=CARTESIAN_POINT('Ctrl Pts',(10.6211545887425,-0.000548317120500629,
4.59406879148573));
#16278=CARTESIAN_POINT('Origin',(4.,0.,4.));
#16279=CARTESIAN_POINT('',(11.0288454112576,0.000503618959454472,4.59367252935801));
#16280=CARTESIAN_POINT('',(10.9211545887425,0.000179316795020235,4.59501533910171));
#16281=CARTESIAN_POINT('',(4.,-7.27562663373442E-17,4.5941));
#16282=CARTESIAN_POINT('Ctrl Pts',(11.0288454112576,0.000503618959454472,
4.59367252935801));
#16283=CARTESIAN_POINT('Ctrl Pts',(11.0239597716647,0.0613870506829751,
4.59415995979602));
#16284=CARTESIAN_POINT('Ctrl Pts',(11.0190741320719,0.122135879976345,4.58554712933309));
#16285=CARTESIAN_POINT('Ctrl Pts',(11.014188492479,0.179818659528701,4.56726203449827));
#16286=CARTESIAN_POINT('Ctrl Pts',(10.9982832137914,0.36760588100072,4.50773461262244));
#16287=CARTESIAN_POINT('Ctrl Pts',(10.9823779351038,0.52289792528528,4.34569680405454));
#16288=CARTESIAN_POINT('Ctrl Pts',(10.9664726564162,0.574391255511512,4.15554951523459));
#16289=CARTESIAN_POINT('Ctrl Pts',(10.9505673777285,0.625884585737745,3.96540222641464));
#16290=CARTESIAN_POINT('Ctrl Pts',(10.9346620990409,0.573579201905647,3.74714545734266));
#16291=CARTESIAN_POINT('Ctrl Pts',(10.9187568203533,0.441491523412615,3.60099348269406));
#16292=CARTESIAN_POINT('Ctrl Pts',(10.9028515416657,0.309403844919578,3.45484150804546));
#16293=CARTESIAN_POINT('Ctrl Pts',(10.8869462629781,0.0975338717655902,
3.38079432782024));
#16294=CARTESIAN_POINT('Ctrl Pts',(10.8710409842905,-0.0968366678563846,
3.41285127449999));
#16295=CARTESIAN_POINT('Ctrl Pts',(10.8551357056029,-0.291207207478354,
3.44490822117975));
#16296=CARTESIAN_POINT('Ctrl Pts',(10.8392304269153,-0.468078313568319,
3.58306929476445));
#16297=CARTESIAN_POINT('Ctrl Pts',(10.8233251482276,-0.546238257009186,
3.76389677537701));
#16298=CARTESIAN_POINT('Ctrl Pts',(10.80741986954,-0.624398200450053,3.94472425598957));
#16299=CARTESIAN_POINT('Ctrl Pts',(10.7915145908524,-0.603846981241821,
4.16821814362997));
#16300=CARTESIAN_POINT('Ctrl Pts',(10.7756093121648,-0.494020849794526,
4.33175950034039));
#16301=CARTESIAN_POINT('Ctrl Pts',(10.7600213451957,-0.386385759396791,
4.49203819249975));
#16302=CARTESIAN_POINT('Ctrl Pts',(10.7444333782267,-0.193002309618558,
4.59473260886404));
#16303=CARTESIAN_POINT('Ctrl Pts',(10.7288454112576,7.37317986114466E-5,
4.59506942345298));
#16304=CARTESIAN_POINT('Ctrl Pts',(10.6211545887425,-0.000548317120500629,
4.59406879148573));
#16305=CARTESIAN_POINT('Ctrl Pts',(10.6249367967398,-0.0476013079303647,
4.5945019577127));
#16306=CARTESIAN_POINT('Ctrl Pts',(10.6287190047372,-0.0945611723716044,
4.58938408097059));
#16307=CARTESIAN_POINT('Ctrl Pts',(10.6325012127345,-0.140089514783682,
4.57835619988505));
#16308=CARTESIAN_POINT('Ctrl Pts',(10.6484064914221,-0.331549364363767,
4.53198076994489));
#16309=CARTESIAN_POINT('Ctrl Pts',(10.6643117701097,-0.497693523030948,
4.38109011760241));
#16310=CARTESIAN_POINT('Ctrl Pts',(10.6802170487973,-0.562235622104956,
4.19496684675621));
#16311=CARTESIAN_POINT('Ctrl Pts',(10.6961223274849,-0.626777721178965,
4.00884357591002));
#16312=CARTESIAN_POINT('Ctrl Pts',(10.7120276061725,-0.589717760659791,
3.78748768656011));
#16313=CARTESIAN_POINT('Ctrl Pts',(10.7279328848602,-0.468072106540212,
3.63253643830059));
#16314=CARTESIAN_POINT('Ctrl Pts',(10.7438381635478,-0.346426452420629,
3.47758519004106));
#16315=CARTESIAN_POINT('Ctrl Pts',(10.7597434422354,-0.140195104700642,
3.38903858287192));
#16316=CARTESIAN_POINT('Ctrl Pts',(10.775648720923,0.0559292266755373,3.40755347270721));
#16317=CARTESIAN_POINT('Ctrl Pts',(10.7915539996106,0.252053558051711,3.4260683625425));
#16318=CARTESIAN_POINT('Ctrl Pts',(10.8074592782982,0.438070873084069,3.55164474938222));
#16319=CARTESIAN_POINT('Ctrl Pts',(10.8233645569858,0.528569890453362,3.72662326908837));
#16320=CARTESIAN_POINT('Ctrl Pts',(10.8392698356734,0.619068907822657,3.90160178879453));
#16321=CARTESIAN_POINT('Ctrl Pts',(10.8551751143611,0.614049627528876,4.12598244136713));
#16322=CARTESIAN_POINT('Ctrl Pts',(10.8710803930487,0.515816690734684,4.29673912390739));
#16323=CARTESIAN_POINT('Ctrl Pts',(10.8869856717363,0.417583753940498,4.46749580644764));
#16324=CARTESIAN_POINT('Ctrl Pts',(10.9028909504239,0.226137160645921,4.58462851895556));
#16325=CARTESIAN_POINT('Ctrl Pts',(10.9187962291115,0.0293810870543861,
4.59435487532392));
#16326=CARTESIAN_POINT('Ctrl Pts',(10.9195823489885,0.0196563998352688,
4.59483560139116));
#16327=CARTESIAN_POINT('Ctrl Pts',(10.9203684688655,0.00991874240631306,
4.5950539509358));
#16328=CARTESIAN_POINT('Ctrl Pts',(10.9211545887425,0.000179316795020235,
4.59501533910171));
#16329=CARTESIAN_POINT('Origin',(4.,0.,4.));
#16330=CARTESIAN_POINT('',(11.3288454112576,-0.000294350894641693,4.59325842069974));
#16331=CARTESIAN_POINT('',(11.2211545887425,0.000456638431143918,4.59352536526061));
#16332=CARTESIAN_POINT('',(4.,-7.27562663373442E-17,4.5941));
#16333=CARTESIAN_POINT('Ctrl Pts',(11.3288454112576,-0.000294350894641693,
4.59325842069974));
#16334=CARTESIAN_POINT('Ctrl Pts',(11.3193914437904,0.117725031793324,4.59273125875086));
#16335=CARTESIAN_POINT('Ctrl Pts',(11.3099374763232,0.236024696118704,4.55868066117597));
#16336=CARTESIAN_POINT('Ctrl Pts',(11.300483508856,0.333060002447629,4.49314500997921));
#16337=CARTESIAN_POINT('Ctrl Pts',(11.2845782301684,0.496311419914153,4.38288835848583));
#16338=CARTESIAN_POINT('Ctrl Pts',(11.2686729514808,0.599375291650127,4.18351506848348));
#16339=CARTESIAN_POINT('Ctrl Pts',(11.2527676727932,0.594929048027223,3.98656891995295));
#16340=CARTESIAN_POINT('Ctrl Pts',(11.2368623941056,0.59048280440432,3.78962277142242));
#16341=CARTESIAN_POINT('Ctrl Pts',(11.220957115418,0.478526445422532,3.5951037643637));
#16342=CARTESIAN_POINT('Ctrl Pts',(11.2050518367303,0.310465594643358,3.49232679739763));
#16343=CARTESIAN_POINT('Ctrl Pts',(11.1891465580427,0.142404743864184,3.38954983043155));
#16344=CARTESIAN_POINT('Ctrl Pts',(11.1732412793551,-0.0817605987123653,
3.37851490355812));
#16345=CARTESIAN_POINT('Ctrl Pts',(11.1573360006675,-0.259103191428711,
3.46428878834836));
#16346=CARTESIAN_POINT('Ctrl Pts',(11.1414307219799,-0.436445784145052,
3.5500626731386));
#16347=CARTESIAN_POINT('Ctrl Pts',(11.1255254432923,-0.566965627001181,
3.73264536959251));
#16348=CARTESIAN_POINT('Ctrl Pts',(11.1096201646047,-0.590733529996744,
3.92820262793532));
#16349=CARTESIAN_POINT('Ctrl Pts',(11.0937148859171,-0.614501432992307,
4.12375988627813));
#16350=CARTESIAN_POINT('Ctrl Pts',(11.0778096072294,-0.531517396127296,
4.33229170650985));
#16351=CARTESIAN_POINT('Ctrl Pts',(11.0619043285418,-0.379884178365051,
4.45804909903384));
#16352=CARTESIAN_POINT('Ctrl Pts',(11.0508846894471,-0.274828280424841,
4.54517747360242));
#16353=CARTESIAN_POINT('Ctrl Pts',(11.0398650503523,-0.136819945681758,
4.59257312212411));
#16354=CARTESIAN_POINT('Ctrl Pts',(11.0288454112576,0.000503618959454472,
4.59367252935801));
#16355=CARTESIAN_POINT('Ctrl Pts',(10.9211545887425,0.000179316795020235,
4.59501533910171));
#16356=CARTESIAN_POINT('Ctrl Pts',(10.9362737475531,-0.187135527734918,
4.59427273168419));
#16357=CARTESIAN_POINT('Ctrl Pts',(10.9513929063637,-0.375104412928531,
4.49848156101044));
#16358=CARTESIAN_POINT('Ctrl Pts',(10.9665120651743,-0.484035620954107,
4.34616539940523));
#16359=CARTESIAN_POINT('Ctrl Pts',(10.982417343862,-0.598630701482551,4.1859295668894));
#16360=CARTESIAN_POINT('Ctrl Pts',(10.9983226225496,-0.625755308650954,
3.96313790162893));
#16361=CARTESIAN_POINT('Ctrl Pts',(11.0142279012372,-0.55295497039508,3.7800869107734));
#16362=CARTESIAN_POINT('Ctrl Pts',(11.0301331799248,-0.480154632139201,
3.59703591991786));
#16363=CARTESIAN_POINT('Ctrl Pts',(11.0460384586124,-0.307429348459053,
3.45372560346725));
#16364=CARTESIAN_POINT('Ctrl Pts',(11.0619437373,-0.114087262216405,3.41595799577618));
#16365=CARTESIAN_POINT('Ctrl Pts',(11.0778490159876,0.0792548240262376,
3.37819038808511));
#16366=CARTESIAN_POINT('Ctrl Pts',(11.0937542946752,0.293213712831377,3.4459654891536));
#16367=CARTESIAN_POINT('Ctrl Pts',(11.1096595733629,0.429548534313776,3.58816383989905));
#16368=CARTESIAN_POINT('Ctrl Pts',(11.1255648520505,0.565883355796175,3.7303621906445));
#16369=CARTESIAN_POINT('Ctrl Pts',(11.1414701307381,0.624594109955846,3.94698379106692));
#16370=CARTESIAN_POINT('Ctrl Pts',(11.1573754094257,0.578723302329844,4.13856516675647));
#16371=CARTESIAN_POINT('Ctrl Pts',(11.1732806881133,0.53285249470384,4.33014654244603));
#16372=CARTESIAN_POINT('Ctrl Pts',(11.1891859668009,0.382400125292158,4.49668769340272));
#16373=CARTESIAN_POINT('Ctrl Pts',(11.2050912454885,0.196447557013804,4.56171996888228));
#16374=CARTESIAN_POINT('Ctrl Pts',(11.2104456932399,0.133847376870746,4.58361282144047));
#16375=CARTESIAN_POINT('Ctrl Pts',(11.2158001409912,0.0672239414478651,
4.5940016224088));
#16376=CARTESIAN_POINT('Ctrl Pts',(11.2211545887425,0.000456638431143918,
4.59352536526061));
#16377=CARTESIAN_POINT('Origin',(4.,0.,4.));
#16378=CARTESIAN_POINT('',(11.6288454112576,-0.000389145320547679,4.59475273347735));
#16379=CARTESIAN_POINT('',(11.5211545887425,-0.0003715675665865,4.59335763259963));
#16380=CARTESIAN_POINT('',(4.,-7.27562663373442E-17,4.5941));
#16381=CARTESIAN_POINT('Ctrl Pts',(11.6288454112576,-0.000389145320547679,
4.59475273347735));
#16382=CARTESIAN_POINT('Ctrl Pts',(11.6148231159161,0.173538999407471,4.59343557735163));
#16383=CARTESIAN_POINT('Ctrl Pts',(11.6008008205746,0.348531733704351,4.51264940831536));
#16384=CARTESIAN_POINT('Ctrl Pts',(11.586778525233,0.459048433726307,4.37867598496766));
#16385=CARTESIAN_POINT('Ctrl Pts',(11.5708732465454,0.584405864209301,4.22671194604376));
#16386=CARTESIAN_POINT('Ctrl Pts',(11.5549679678578,0.626808276394098,4.00631705984067));
#16387=CARTESIAN_POINT('Ctrl Pts',(11.5390626891702,0.566786276503563,3.81868733396413));
#16388=CARTESIAN_POINT('Ctrl Pts',(11.5231574104826,0.506764276613028,3.6310576080876));
#16389=CARTESIAN_POINT('Ctrl Pts',(11.507252131795,0.344317864647159,3.47619304253762));
#16390=CARTESIAN_POINT('Ctrl Pts',(11.4913468531074,0.154035560439752,3.4252008940353));
#16391=CARTESIAN_POINT('Ctrl Pts',(11.4754415744198,-0.0362467437676612,
3.37420874553297));
#16392=CARTESIAN_POINT('Ctrl Pts',(11.4595362957322,-0.254364940216614,
3.4270890140783));
#16393=CARTESIAN_POINT('Ctrl Pts',(11.4436310170445,-0.400168380917644,
3.55956131753494));
#16394=CARTESIAN_POINT('Ctrl Pts',(11.4277257383569,-0.545971821618673,
3.69203362099157));
#16395=CARTESIAN_POINT('Ctrl Pts',(11.4118204596693,-0.619460506571779,
3.90409795935952));
#16396=CARTESIAN_POINT('Ctrl Pts',(11.3959151809817,-0.586891540696359,
4.09838336016249));
#16397=CARTESIAN_POINT('Ctrl Pts',(11.3800099022941,-0.554322574820941,
4.29266876096545));
#16398=CARTESIAN_POINT('Ctrl Pts',(11.3641046236065,-0.415695958117004,
4.46917522420345));
#16399=CARTESIAN_POINT('Ctrl Pts',(11.3481993449189,-0.234663168166497,
4.54685844933023));
#16400=CARTESIAN_POINT('Ctrl Pts',(11.3417480336984,-0.161234786808821,
4.57836740127901));
#16401=CARTESIAN_POINT('Ctrl Pts',(11.335296722478,-0.080829826651965,4.59361815176584));
#16402=CARTESIAN_POINT('Ctrl Pts',(11.3288454112576,-0.000294350894641693,
4.59325842069974));
#16403=CARTESIAN_POINT('Ctrl Pts',(11.2211545887425,0.000456638431143918,
4.59352536526061));
#16404=CARTESIAN_POINT('Ctrl Pts',(11.2317054196788,-0.131106980996848,
4.59258691018808));
#16405=CARTESIAN_POINT('Ctrl Pts',(11.2422562506151,-0.263229208150973,
4.54946171071576));
#16406=CARTESIAN_POINT('Ctrl Pts',(11.2528070815514,-0.366229002642205,
4.4690386804108));
#16407=CARTESIAN_POINT('Ctrl Pts',(11.268712360239,-0.521500226874852,4.34780171645731));
#16408=CARTESIAN_POINT('Ctrl Pts',(11.2846176389266,-0.610589908195122,
4.1418043885479));
#16409=CARTESIAN_POINT('Ctrl Pts',(11.3005229176142,-0.592591834014348,
3.94563195463032));
#16410=CARTESIAN_POINT('Ctrl Pts',(11.3164281963018,-0.574593759833574,
3.74945952071274));
#16411=CARTESIAN_POINT('Ctrl Pts',(11.3323334749894,-0.449507930151742,
3.56311198078699));
#16412=CARTESIAN_POINT('Ctrl Pts',(11.3482387536771,-0.274768466013715,
3.47215224147272));
#16413=CARTESIAN_POINT('Ctrl Pts',(11.3641440323647,-0.100029001875688,
3.38119250215845));
#16414=CARTESIAN_POINT('Ctrl Pts',(11.3800493110523,0.12436409671854,3.38562056345565));
#16415=CARTESIAN_POINT('Ctrl Pts',(11.3959545897399,0.295379012183608,3.48340324695247));
#16416=CARTESIAN_POINT('Ctrl Pts',(11.4118598684275,0.466393927648671,3.5811859304493));
#16417=CARTESIAN_POINT('Ctrl Pts',(11.4277651471151,0.584030659984583,3.77232323614575));
#16418=CARTESIAN_POINT('Ctrl Pts',(11.4436704258027,0.594275398502411,3.96905299961855));
#16419=CARTESIAN_POINT('Ctrl Pts',(11.4595757044903,0.60452013702024,4.16578276309136));
#16420=CARTESIAN_POINT('Ctrl Pts',(11.475480983178,0.507372881719984,4.36810498434052));
#16421=CARTESIAN_POINT('Ctrl Pts',(11.4913862618656,0.34743954227408,4.48312185891572));
#16422=CARTESIAN_POINT('Ctrl Pts',(11.5013090374912,0.247662438486696,4.55487707062799));
#16423=CARTESIAN_POINT('Ctrl Pts',(11.5112318131169,0.123448374926332,4.59265218509947));
#16424=CARTESIAN_POINT('Ctrl Pts',(11.5211545887425,-0.0003715675665865,
4.59335763259963));
#16425=CARTESIAN_POINT('Origin',(4.,0.,4.));
#16426=CARTESIAN_POINT('',(11.9288454112576,0.000492284285450728,4.5944814532616));
#16427=CARTESIAN_POINT('',(11.8211545887425,-0.000307672146732893,4.59488449882539));
#16428=CARTESIAN_POINT('',(4.,-7.27562663373442E-17,4.5941));
#16429=CARTESIAN_POINT('Ctrl Pts',(11.9288454112576,0.000492284285450728,
4.5944814532616));
#16430=CARTESIAN_POINT('Ctrl Pts',(11.9261600667293,0.0338400408399785,
4.59477876231094));
#16431=CARTESIAN_POINT('Ctrl Pts',(11.9234747222011,0.0671420792079604,
4.59221542322669));
#16432=CARTESIAN_POINT('Ctrl Pts',(11.9207893776729,0.0999293694653808,
4.5866302815369));
#16433=CARTESIAN_POINT('Ctrl Pts',(11.9048840989853,0.294128282668868,4.55354952256816));
#16434=CARTESIAN_POINT('Ctrl Pts',(11.8889788202977,0.470268877700486,4.41445832512751));
#16435=CARTESIAN_POINT('Ctrl Pts',(11.8730735416101,0.547474845215755,4.2332214826164));
#16436=CARTESIAN_POINT('Ctrl Pts',(11.8571682629225,0.624680812731027,4.05198464010529));
#16437=CARTESIAN_POINT('Ctrl Pts',(11.8412629842349,0.602952152729945,3.82860215252373));
#16438=CARTESIAN_POINT('Ctrl Pts',(11.8253577055472,0.492265746621211,3.66564180763548));
#16439=CARTESIAN_POINT('Ctrl Pts',(11.8094524268596,0.38157934051248,3.50268146274723));
#16440=CARTESIAN_POINT('Ctrl Pts',(11.793547148172,0.181935188296101,3.40014326055229));
#16441=CARTESIAN_POINT('Ctrl Pts',(11.7776418694844,-0.0149985615777061,
3.40510840546499));
#16442=CARTESIAN_POINT('Ctrl Pts',(11.7617365907968,-0.211932311451519,
3.41007355037768));
#16443=CARTESIAN_POINT('Ctrl Pts',(11.7458313121092,-0.406155658982761,
3.52254204239802));
#16444=CARTESIAN_POINT('Ctrl Pts',(11.7299260334216,-0.508489459897291,
3.69087310813977));
#16445=CARTESIAN_POINT('Ctrl Pts',(11.714020754734,-0.610823260811815,3.8592041738815));
#16446=CARTESIAN_POINT('Ctrl Pts',(11.6981154760463,-0.621267515109637,
4.08339781334463));
#16447=CARTESIAN_POINT('Ctrl Pts',(11.6822101973587,-0.53502666307716,4.26051379213839));
#16448=CARTESIAN_POINT('Ctrl Pts',(11.6663049186711,-0.448785811044678,
4.43762977093217));
#16449=CARTESIAN_POINT('Ctrl Pts',(11.6503996399835,-0.265859852681883,
4.56766808905658));
#16450=CARTESIAN_POINT('Ctrl Pts',(11.6344943612959,-0.070240649109886,
4.59092065229643));
#16451=CARTESIAN_POINT('Ctrl Pts',(11.6326113779498,-0.0470818155087989,
4.59367346098309));
#16452=CARTESIAN_POINT('Ctrl Pts',(11.6307283946037,-0.0237450789937817,
4.59492960773286));
#16453=CARTESIAN_POINT('Ctrl Pts',(11.6288454112576,-0.000389145320547679,
4.59475273347735));
#16454=CARTESIAN_POINT('Ctrl Pts',(11.5211545887425,-0.0003715675665865,
4.59335763259963));
#16455=CARTESIAN_POINT('Ctrl Pts',(11.5271370918045,-0.0750233800274846,
4.5937829512795));
#16456=CARTESIAN_POINT('Ctrl Pts',(11.5331195948664,-0.149531931096223,
4.58073359799715));
#16457=CARTESIAN_POINT('Ctrl Pts',(11.5391020979284,-0.218455391669058,
4.55353248138526));
#16458=CARTESIAN_POINT('Ctrl Pts',(11.555007376616,-0.40169756257477,4.48121470137836));
#16459=CARTESIAN_POINT('Ctrl Pts',(11.5709126553036,-0.545462480794654,
4.3088676134633));
#16460=CARTESIAN_POINT('Ctrl Pts',(11.5868179339912,-0.583739378074245,
4.1156257090067));
#16461=CARTESIAN_POINT('Ctrl Pts',(11.6027232126789,-0.622016275353834,
3.92238380455011));
#16462=CARTESIAN_POINT('Ctrl Pts',(11.6186284913665,-0.554805151693135,
3.70824708355197));
#16463=CARTESIAN_POINT('Ctrl Pts',(11.6345337700541,-0.412966511608993,
3.57153806891708));
#16464=CARTESIAN_POINT('Ctrl Pts',(11.6504390487417,-0.271127871524847,
3.43482905428217));
#16465=CARTESIAN_POINT('Ctrl Pts',(11.6663443274293,-0.0546617150172531,
3.37554774601052));
#16466=CARTESIAN_POINT('Ctrl Pts',(11.6822496061169,0.137039856773353,3.42091361287512));
#16467=CARTESIAN_POINT('Ctrl Pts',(11.6981548848045,0.328741428563947,3.46627947973972));
#16468=CARTESIAN_POINT('Ctrl Pts',(11.7140601634921,0.495678415637556,3.61629252174057));
#16469=CARTESIAN_POINT('Ctrl Pts',(11.7299654421798,0.56120041605148,3.80207309651931));
#16470=CARTESIAN_POINT('Ctrl Pts',(11.7458707208674,0.626722416465409,3.98785367129807));
#16471=CARTESIAN_POINT('Ctrl Pts',(11.761775999555,0.590829430219633,4.20940177885472));
#16472=CARTESIAN_POINT('Ctrl Pts',(11.7776812782426,0.470001998091193,4.36499190112672));
#16473=CARTESIAN_POINT('Ctrl Pts',(11.7921723817426,0.359917612963646,4.5067481450567));
#16474=CARTESIAN_POINT('Ctrl Pts',(11.8066634852425,0.179330777996457,4.59375393408315));
#16475=CARTESIAN_POINT('Ctrl Pts',(11.8211545887425,-0.000307672146732893,
4.59488449882539));
#16476=CARTESIAN_POINT('Origin',(4.,0.,4.));
#16477=CARTESIAN_POINT('',(12.2288454112576,0.000142795628640946,4.59314744373127));
#16478=CARTESIAN_POINT('',(12.1211545887425,0.00052868291625318,4.59430727435519));
#16479=CARTESIAN_POINT('',(4.,-7.27562663373442E-17,4.5941));
#16480=CARTESIAN_POINT('Ctrl Pts',(12.2288454112576,0.000142795628640946,
4.59314744373127));
#16481=CARTESIAN_POINT('Ctrl Pts',(12.221591738855,0.0907369315914116,4.59334157666405));
#16482=CARTESIAN_POINT('Ctrl Pts',(12.2143380664525,0.181251971066953,4.57388161006077));
#16483=CARTESIAN_POINT('Ctrl Pts',(12.2070843940499,0.261922584292681,4.53433840020651));
#16484=CARTESIAN_POINT('Ctrl Pts',(12.1911791153623,0.438810719578057,4.44763117963851));
#16485=CARTESIAN_POINT('Ctrl Pts',(12.1752738366747,0.56836661021043,4.26436322928705));
#16486=CARTESIAN_POINT('Ctrl Pts',(12.1593685579871,0.591103672269137,4.06868343852597));
#16487=CARTESIAN_POINT('Ctrl Pts',(12.1434632792995,0.613840734327844,3.87300364776488));
#16488=CARTESIAN_POINT('Ctrl Pts',(12.1275580006119,0.529758967812885,3.66491201659415));
#16489=CARTESIAN_POINT('Ctrl Pts',(12.1116527219243,0.377465162701742,3.53995541841648));
#16490=CARTESIAN_POINT('Ctrl Pts',(12.0957474432367,0.225171357590603,3.41499882023882));
#16491=CARTESIAN_POINT('Ctrl Pts',(12.0798421645491,0.00466551388328543,
3.37317725505421));
#16492=CARTESIAN_POINT('Ctrl Pts',(12.0639368858614,-0.182805413822737,
3.43369341627091));
#16493=CARTESIAN_POINT('Ctrl Pts',(12.0480316071738,-0.37027634152876,3.49420957748762));
#16494=CARTESIAN_POINT('Ctrl Pts',(12.0321263284862,-0.524712353233489,
3.65706346510565));
#16495=CARTESIAN_POINT('Ctrl Pts',(12.0162210497986,-0.575202966010955,
3.84747946371059));
#16496=CARTESIAN_POINT('Ctrl Pts',(12.000315771111,-0.625693578788423,4.03789546231555));
#16497=CARTESIAN_POINT('Ctrl Pts',(11.9844104924234,-0.572238792638624,
4.25587357190742));
#16498=CARTESIAN_POINT('Ctrl Pts',(11.9685052137358,-0.439382783876041,
4.40132746645495));
#16499=CARTESIAN_POINT('Ctrl Pts',(11.9552852795764,-0.328957325572706,
4.52222386487166));
#16500=CARTESIAN_POINT('Ctrl Pts',(11.942065345417,-0.163678510702966,4.59301780268865));
#16501=CARTESIAN_POINT('Ctrl Pts',(11.9288454112576,0.000492284285450728,
4.5944814532616));
#16502=CARTESIAN_POINT('Ctrl Pts',(11.8211545887425,-0.000307672146732893,
4.59488449882539));
#16503=CARTESIAN_POINT('Ctrl Pts',(11.8225687639301,-0.0178384446610953,
4.59499482973335));
#16504=CARTESIAN_POINT('Ctrl Pts',(11.8239829391178,-0.035360185088601,
4.59428731490513));
#16505=CARTESIAN_POINT('Ctrl Pts',(11.8253971143054,-0.0528064866265509,
4.59273302680715));
#16506=CARTESIAN_POINT('Ctrl Pts',(11.8413023929931,-0.249025661204777,
4.57525189322826));
#16507=CARTESIAN_POINT('Ctrl Pts',(11.8572076716807,-0.435702132350142,
4.45065748908313));
#16508=CARTESIAN_POINT('Ctrl Pts',(11.8731129503683,-0.527121962142897,
4.27615829360067));
#16509=CARTESIAN_POINT('Ctrl Pts',(11.8890182290559,-0.618541791935657,
4.10165909811819));
#16510=CARTESIAN_POINT('Ctrl Pts',(11.9049235077435,-0.614704980375792,
3.87725511129838));
#16511=CARTESIAN_POINT('Ctrl Pts',(11.9208287864311,-0.517373229009482,
3.70598315013913));
#16512=CARTESIAN_POINT('Ctrl Pts',(11.9367340651187,-0.420041477643178,
3.53471118897989));
#16513=CARTESIAN_POINT('Ctrl Pts',(11.9526393438063,-0.229214786470442,
3.41657125348121));
#16514=CARTESIAN_POINT('Ctrl Pts',(11.9685446224939,-0.0325126988662629,
3.4058082039356));
#16515=CARTESIAN_POINT('Ctrl Pts',(11.9844499011816,0.164189388737916,3.39504515438998));
#16516=CARTESIAN_POINT('Ctrl Pts',(12.0003551798692,0.366766872773537,3.49165899079743));
#16517=CARTESIAN_POINT('Ctrl Pts',(12.0162604585568,0.482204742918021,3.65128872687397));
#16518=CARTESIAN_POINT('Ctrl Pts',(12.0321657372444,0.597642613062508,3.81091846295053));
#16519=CARTESIAN_POINT('Ctrl Pts',(12.048071015932,0.625940869315854,4.03356409869619));
#16520=CARTESIAN_POINT('Ctrl Pts',(12.0639762946196,0.554106149607013,4.21699617753661));
#16521=CARTESIAN_POINT('Ctrl Pts',(12.0798815733072,0.482271429898174,4.40042825637702));
#16522=CARTESIAN_POINT('Ctrl Pts',(12.0957868519948,0.310303734227154,4.5446467783122));
#16523=CARTESIAN_POINT('Ctrl Pts',(12.1116921306825,0.117163353092859,4.583432699452));
#16524=CARTESIAN_POINT('Ctrl Pts',(12.1148462833691,0.0788619649798074,
4.59112427906975));
#16525=CARTESIAN_POINT('Ctrl Pts',(12.1180004360558,0.0397279339241207,
4.59466958677844));
#16526=CARTESIAN_POINT('Ctrl Pts',(12.1211545887425,0.00052868291625318,
4.59430727435519));
#16527=CARTESIAN_POINT('Origin',(4.,0.,4.));
#16528=CARTESIAN_POINT('',(12.5288454112576,-0.000545899910317726,4.59395595168017));
#16529=CARTESIAN_POINT('',(12.4211545887425,4.74932194801069E-5,4.59311952367199));
#16530=CARTESIAN_POINT('',(4.,-7.27562663373442E-17,4.5941));
#16531=CARTESIAN_POINT('Ctrl Pts',(12.5288454112576,-0.000545899910317726,
4.59395595168017));
#16532=CARTESIAN_POINT('Ctrl Pts',(12.5170234109807,0.14659828900878,4.5926299020853));
#16533=CARTESIAN_POINT('Ctrl Pts',(12.5052014107038,0.29463204299547,4.53735693360054));
#16534=CARTESIAN_POINT('Ctrl Pts',(12.493379410427,0.402483765871145,4.43832383497591));
#16535=CARTESIAN_POINT('Ctrl Pts',(12.4774741317394,0.547587104485886,4.30508504322883));
#16536=CARTESIAN_POINT('Ctrl Pts',(12.4615688530518,0.619957272242066,4.09263639239171));
#16537=CARTESIAN_POINT('Ctrl Pts',(12.4456635743641,0.586364949835353,3.89852531496775));
#16538=CARTESIAN_POINT('Ctrl Pts',(12.4297582956765,0.55277262742864,3.7044142375438));
#16539=CARTESIAN_POINT('Ctrl Pts',(12.4138530169889,0.41321781485904,3.52864073353302));
#16540=CARTESIAN_POINT('Ctrl Pts',(12.3979477383013,0.231778177981285,3.45191255961345));
#16541=CARTESIAN_POINT('Ctrl Pts',(12.3820424596137,0.0503385411035255,
3.37518438569388));
#16542=CARTESIAN_POINT('Ctrl Pts',(12.3661371809261,-0.172985920082391,
3.39750154186552));
#16543=CARTESIAN_POINT('Ctrl Pts',(12.3502319022385,-0.335654061078685,
3.50861693417539));
#16544=CARTESIAN_POINT('Ctrl Pts',(12.3343266235509,-0.498322202074975,
3.61973232648525));
#16545=CARTESIAN_POINT('Ctrl Pts',(12.3184213448632,-0.600334022881645,
3.81964595493332));
#16546=CARTESIAN_POINT('Ctrl Pts',(12.3025160661756,-0.594850011148503,
4.0165659389844));
#16547=CARTESIAN_POINT('Ctrl Pts',(12.286610787488,-0.58936599941536,4.21348592303547));
#16548=CARTESIAN_POINT('Ctrl Pts',(12.2707055088004,-0.476386155142398,
4.40741226268955));
#16549=CARTESIAN_POINT('Ctrl Pts',(12.2548002301128,-0.307786043036728,
4.50930218712431));
#16550=CARTESIAN_POINT('Ctrl Pts',(12.2461486238277,-0.216076754679914,
4.564724762732));
#16551=CARTESIAN_POINT('Ctrl Pts',(12.2374970175426,-0.107910718865932,
4.59291589733543));
#16552=CARTESIAN_POINT('Ctrl Pts',(12.2288454112576,0.000142795628640946,
4.59314744373127));
#16553=CARTESIAN_POINT('Ctrl Pts',(12.1211545887425,0.00052868291625318,
4.59430727435519));
#16554=CARTESIAN_POINT('Ctrl Pts',(12.1339057147434,-0.157940052872902,
4.59284257311225));
#16555=CARTESIAN_POINT('Ctrl Pts',(12.1466568407444,-0.317474678016714,
4.52751565545538));
#16556=CARTESIAN_POINT('Ctrl Pts',(12.1594079667453,-0.427372353356377,
4.41409399619463));
#16557=CARTESIAN_POINT('Ctrl Pts',(12.1753132454329,-0.564454612073754,
4.27261605145303));
#16558=CARTESIAN_POINT('Ctrl Pts',(12.1912185241205,-0.62430606291093,4.0563068416254));
#16559=CARTESIAN_POINT('Ctrl Pts',(12.2071238028081,-0.579445451749542,
3.8644864045766));
#16560=CARTESIAN_POINT('Ctrl Pts',(12.2230290814957,-0.534584840588155,
3.6726659675278));
#16561=CARTESIAN_POINT('Ctrl Pts',(12.2389343601834,-0.38501216742821,3.50533430325784));
#16562=CARTESIAN_POINT('Ctrl Pts',(12.254839638871,-0.199404875886796,3.43932303278057));
#16563=CARTESIAN_POINT('Ctrl Pts',(12.2707449175586,-0.0137975843453769,
3.37331176230329));
#16564=CARTESIAN_POINT('Ctrl Pts',(12.2866501962462,0.207844325577514,3.40862088561871));
#16565=CARTESIAN_POINT('Ctrl Pts',(12.3025554749338,0.363752265741203,3.52903794710619));
#16566=CARTESIAN_POINT('Ctrl Pts',(12.3184607536214,0.519660205904889,3.64945500859368));
#16567=CARTESIAN_POINT('Ctrl Pts',(12.334366032309,0.609834176309377,3.85498000825323));
#16568=CARTESIAN_POINT('Ctrl Pts',(12.3502713109967,0.592870104691008,4.05124456128685));
#16569=CARTESIAN_POINT('Ctrl Pts',(12.3661765896843,0.575906033072638,4.24750911432049));
#16570=CARTESIAN_POINT('Ctrl Pts',(12.3820818683719,0.451803919431404,4.4345132207282));
#16571=CARTESIAN_POINT('Ctrl Pts',(12.3979871470595,0.277546204023914,4.52639250633888));
#16572=CARTESIAN_POINT('Ctrl Pts',(12.4057096276205,0.192938958450368,4.57100260157974));
#16573=CARTESIAN_POINT('Ctrl Pts',(12.4134321081815,0.0965080911524262,
4.59318808505049));
#16574=CARTESIAN_POINT('Ctrl Pts',(12.4211545887425,4.74932194801069E-5,
4.59311952367199));
#16575=CARTESIAN_POINT('Origin',(4.,0.,4.));
#16576=CARTESIAN_POINT('',(12.8288454112576,0.000112157221815526,4.59505491513413));
#16577=CARTESIAN_POINT('',(12.7211545887425,-0.000546355209092884,4.59413239245978));
#16578=CARTESIAN_POINT('',(4.,-7.27562663373442E-17,4.5941));
#16579=CARTESIAN_POINT('Ctrl Pts',(12.8288454112576,0.000112157221815526,
4.59505491513413));
#16580=CARTESIAN_POINT('Ctrl Pts',(12.828360361794,0.00612048155630211,
4.59507046002904));
#16581=CARTESIAN_POINT('Ctrl Pts',(12.8278753123304,0.0121283652366354,
4.59498736156652));
#16582=CARTESIAN_POINT('Ctrl Pts',(12.8273902628668,0.0181332013859869,
4.59480429815638));
#16583=CARTESIAN_POINT('Ctrl Pts',(12.8114849841792,0.215038052543873,4.58880145767424));
#16584=CARTESIAN_POINT('Ctrl Pts',(12.7955797054916,0.408666038032992,4.47531104548453));
#16585=CARTESIAN_POINT('Ctrl Pts',(12.779674426804,0.510111378641258,4.30644305748136));
#16586=CARTESIAN_POINT('Ctrl Pts',(12.7637691481164,0.611556719249521,4.1375750694782));
#16587=CARTESIAN_POINT('Ctrl Pts',(12.7478638694288,0.620819414976937,3.9133295056616));
#16588=CARTESIAN_POINT('Ctrl Pts',(12.7319585907412,0.533646427817818,3.7366704418887));
#16589=CARTESIAN_POINT('Ctrl Pts',(12.7160533120536,0.446473440658691,3.56001137811579));
#16590=CARTESIAN_POINT('Ctrl Pts',(12.700148033366,0.26286477061301,3.43093881438659));
#16591=CARTESIAN_POINT('Ctrl Pts',(12.6842427546783,0.0671257511235207,
3.4087174113557));
#16592=CARTESIAN_POINT('Ctrl Pts',(12.6683374759907,-0.128613268365957,
3.38649600832481));
#16593=CARTESIAN_POINT('Ctrl Pts',(12.6524321973031,-0.336482637299241,
3.47112576599221));
#16594=CARTESIAN_POINT('Ctrl Pts',(12.6365269186155,-0.461037535689932,
3.62374828002683));
#16595=CARTESIAN_POINT('Ctrl Pts',(12.6206216399279,-0.585592434080627,
3.77637079406146));
#16596=CARTESIAN_POINT('Ctrl Pts',(12.6047163612403,-0.626832861928724,
3.9969860644633));
#16597=CARTESIAN_POINT('Ctrl Pts',(12.5888110825527,-0.565822959504995,
4.18429689252621));
#16598=CARTESIAN_POINT('Ctrl Pts',(12.5729058038651,-0.504813057081268,
4.37160772058911));
#16599=CARTESIAN_POINT('Ctrl Pts',(12.5570005251774,-0.341552824385721,
4.52561410631309));
#16600=CARTESIAN_POINT('Ctrl Pts',(12.5410952464898,-0.151004453301302,
4.57560283284656));
#16601=CARTESIAN_POINT('Ctrl Pts',(12.5370119680791,-0.102085973774189,
4.58843617527608));
#16602=CARTESIAN_POINT('Ctrl Pts',(12.5329286896683,-0.0513689988622793,
4.59441396466913));
#16603=CARTESIAN_POINT('Ctrl Pts',(12.5288454112576,-0.000545899910317726,
4.59395595168017));
#16604=CARTESIAN_POINT('Ctrl Pts',(12.4211545887425,4.74932194801069E-5,
4.59311952367199));
#16605=CARTESIAN_POINT('Ctrl Pts',(12.4293373868691,-0.102162877376194,
4.59304687552285));
#16606=CARTESIAN_POINT('Ctrl Pts',(12.4375201849957,-0.204406628577491,
4.5679880979308));
#16607=CARTESIAN_POINT('Ctrl Pts',(12.4457029831223,-0.292652646395614,
4.51814611323009));
#16608=CARTESIAN_POINT('Ctrl Pts',(12.4616082618099,-0.46418046423393,4.42126596969699));
#16609=CARTESIAN_POINT('Ctrl Pts',(12.4775135404976,-0.582822782736806,
4.23075121781716));
#16610=CARTESIAN_POINT('Ctrl Pts',(12.4934188191852,-0.594104068590283,
4.03407817163935));
#16611=CARTESIAN_POINT('Ctrl Pts',(12.5093240978728,-0.605385354443759,
3.83740512546155));
#16612=CARTESIAN_POINT('Ctrl Pts',(12.5252293765604,-0.509305607647849,
3.63457378498577));
#16613=CARTESIAN_POINT('Ctrl Pts',(12.541134655248,-0.34998058313236,3.51871572067214));
#16614=CARTESIAN_POINT('Ctrl Pts',(12.5570399339356,-0.19065555861687,3.4028576563585));
#16615=CARTESIAN_POINT('Ctrl Pts',(12.5729452126232,0.031914743618199,3.37397286820701));
#16616=CARTESIAN_POINT('Ctrl Pts',(12.5888504913108,0.215535456959467,3.44532402892222));
#16617=CARTESIAN_POINT('Ctrl Pts',(12.6047557699985,0.399156170300736,3.51667518963742));
#16618=CARTESIAN_POINT('Ctrl Pts',(12.6206610486861,0.543827294748204,3.68826229921932));
#16619=CARTESIAN_POINT('Ctrl Pts',(12.6365663273737,0.583121970486127,3.88129981619987));
#16620=CARTESIAN_POINT('Ctrl Pts',(12.6524716060613,0.622416646224052,4.07433733318042));
#16621=CARTESIAN_POINT('Ctrl Pts',(12.6683768847489,0.556334873252426,4.28882525755962));
#16622=CARTESIAN_POINT('Ctrl Pts',(12.6842821634365,0.415218606030559,4.42627980869829));
#16623=CARTESIAN_POINT('Ctrl Pts',(12.6965729718718,0.306170972122536,4.53249785050629));
#16624=CARTESIAN_POINT('Ctrl Pts',(12.7088637803072,0.152317016475741,4.59271595401221));
#16625=CARTESIAN_POINT('Ctrl Pts',(12.7211545887425,-0.000546355209092884,
4.59413239245978));
#16626=CARTESIAN_POINT('Origin',(4.,0.,4.));
#16627=CARTESIAN_POINT('',(13.1288454112576,0.000488576923893258,4.59361798633976));
#16628=CARTESIAN_POINT('',(13.0211545887425,0.000215375668158819,4.59498635240753));
#16629=CARTESIAN_POINT('',(4.,-7.27562663373442E-17,4.5941));
#16630=CARTESIAN_POINT('Ctrl Pts',(13.1288454112576,0.000488576923893258,
4.59361798633976));
#16631=CARTESIAN_POINT('Ctrl Pts',(13.1237920339197,0.0634769139372694,
4.59410397103046));
#16632=CARTESIAN_POINT('Ctrl Pts',(13.1187386565818,0.126326538027094,4.58487602541266));
#16633=CARTESIAN_POINT('Ctrl Pts',(13.1136852792439,0.185787091792062,4.56533540718874));
#16634=CARTESIAN_POINT('Ctrl Pts',(13.0977800005563,0.372936519850693,4.50383218710482));
#16635=CARTESIAN_POINT('Ctrl Pts',(13.0818747218686,0.526512210440984,4.34016674272733));
#16636=CARTESIAN_POINT('Ctrl Pts',(13.065969443181,0.575998703695535,4.14948732200047));
#16637=CARTESIAN_POINT('Ctrl Pts',(13.0500641644934,0.625485196950086,3.9588079012736));
#16638=CARTESIAN_POINT('Ctrl Pts',(13.0341588858058,0.570882492868891,3.74111450419737));
#16639=CARTESIAN_POINT('Ctrl Pts',(13.0182536071182,0.437261843116128,3.59636272886105));
#16640=CARTESIAN_POINT('Ctrl Pts',(13.0023483284306,0.303641193363369,3.45161095352474));
#16641=CARTESIAN_POINT('Ctrl Pts',(12.986443049743,0.0910025979390456,3.37980079992835));
#16642=CARTESIAN_POINT('Ctrl Pts',(12.9705377710554,-0.10301929613509,3.41390445256627));
#16643=CARTESIAN_POINT('Ctrl Pts',(12.9546324923678,-0.297041190209231,
3.4480081052042));
#16644=CARTESIAN_POINT('Ctrl Pts',(12.9387272136801,-0.472446382933184,
3.58802556407645));
#16645=CARTESIAN_POINT('Ctrl Pts',(12.9228219349925,-0.54869623058984,3.76966673571907));
#16646=CARTESIAN_POINT('Ctrl Pts',(12.9069166563049,-0.624946078246494,
3.95130790736168));
#16647=CARTESIAN_POINT('Ctrl Pts',(12.8910113776173,-0.602040580835857,
4.17457279177466));
#16648=CARTESIAN_POINT('Ctrl Pts',(12.8751060989297,-0.490496973717212,
4.33694759959386));
#16649=CARTESIAN_POINT('Ctrl Pts',(12.8596858697056,-0.382355015061345,
4.49437060399126));
#16650=CARTESIAN_POINT('Ctrl Pts',(12.8442656404816,-0.190898750836606,
4.59456072668396));
#16651=CARTESIAN_POINT('Ctrl Pts',(12.8288454112576,0.000112157221815526,
4.59505491513413));
#16652=CARTESIAN_POINT('Ctrl Pts',(12.7211545887425,-0.000546355209092884,
4.59413239245978));
#16653=CARTESIAN_POINT('Ctrl Pts',(12.7247690589948,-0.0455002825709059,
4.59454893744622));
#16654=CARTESIAN_POINT('Ctrl Pts',(12.7283835292471,-0.0903685417208244,
4.58988016539195));
#16655=CARTESIAN_POINT('Ctrl Pts',(12.7319979994994,-0.13398639330236,4.5798004937111));
#16656=CARTESIAN_POINT('Ctrl Pts',(12.747903278187,-0.325924363941296,4.53544544968711));
#16657=CARTESIAN_POINT('Ctrl Pts',(12.7638085568746,-0.493649543747071,
4.38631418374101));
#16658=CARTESIAN_POINT('Ctrl Pts',(12.7797138355622,-0.560149626020051,
4.20088146397168));
#16659=CARTESIAN_POINT('Ctrl Pts',(12.7956191142498,-0.626649708293032,
4.01544874420235));
#16660=CARTESIAN_POINT('Ctrl Pts',(12.8115243929374,-0.591924693033219,
3.79371457060979));
#16661=CARTESIAN_POINT('Ctrl Pts',(12.827429671625,-0.471918838153678,3.63748989490844));
#16662=CARTESIAN_POINT('Ctrl Pts',(12.8433349503126,-0.351912983274129,
3.48126521920708));
#16663=CARTESIAN_POINT('Ctrl Pts',(12.8592402290002,-0.146626288774854,
3.39055004139693));
#16664=CARTESIAN_POINT('Ctrl Pts',(12.8751455076879,0.0496822801939141,
3.40699693328572));
#16665=CARTESIAN_POINT('Ctrl Pts',(12.8910507863755,0.245990849162665,3.42344382517451));
#16666=CARTESIAN_POINT('Ctrl Pts',(12.9069560650631,0.433321292600904,3.54705278676224));
#16667=CARTESIAN_POINT('Ctrl Pts',(12.9228613437507,0.525659396179275,3.72106781235173));
#16668=CARTESIAN_POINT('Ctrl Pts',(12.9387666224383,0.617997499757654,3.89508283794124));
#16669=CARTESIAN_POINT('Ctrl Pts',(12.9546719011259,0.615343263476151,4.11950392753251));
#16670=CARTESIAN_POINT('Ctrl Pts',(12.9705771798135,0.518915400343756,4.29128641125856));
#16671=CARTESIAN_POINT('Ctrl Pts',(12.9864824585012,0.422487537211366,4.46306889498459));
#16672=CARTESIAN_POINT('Ctrl Pts',(13.0023877371888,0.232286047228094,4.58221277284539));
#16673=CARTESIAN_POINT('Ctrl Pts',(13.0182930158764,0.0356434078328121,
4.59401221668908));
#16674=CARTESIAN_POINT('Ctrl Pts',(13.0192468734984,0.0238505254767134,
4.59471984273368));
#16675=CARTESIAN_POINT('Ctrl Pts',(13.0202007311205,0.0120344772878951,
4.59504140054066));
#16676=CARTESIAN_POINT('Ctrl Pts',(13.0211545887425,0.000215375668158819,
4.59498635240753));
#16677=CARTESIAN_POINT('Origin',(4.,0.,4.));
#16678=CARTESIAN_POINT('',(13.4288454112576,-0.000323145728561625,4.59329116515504));
#16679=CARTESIAN_POINT('',(13.3211545887425,0.000436239896754628,4.59347700091179));
#16680=CARTESIAN_POINT('',(4.,-7.27562663373442E-17,4.5941));
#16681=CARTESIAN_POINT('Ctrl Pts',(13.4288454112576,-0.000323145728561625,
4.59329116515504));
#16682=CARTESIAN_POINT('Ctrl Pts',(13.4192237060453,0.11977362227264,4.59270025156928));
#16683=CARTESIAN_POINT('Ctrl Pts',(13.4096020008331,0.240190260834984,4.55734300206483));
#16684=CARTESIAN_POINT('Ctrl Pts',(13.3999802956209,0.338238798929947,4.48960747645051));
#16685=CARTESIAN_POINT('Ctrl Pts',(13.3840750169333,0.500319146323361,4.37763642888821));
#16686=CARTESIAN_POINT('Ctrl Pts',(13.3681697382457,0.601276083433826,4.17718801339723));
#16687=CARTESIAN_POINT('Ctrl Pts',(13.3522644595581,0.594754455875995,3.9802996620979));
#16688=CARTESIAN_POINT('Ctrl Pts',(13.3363591808704,0.588232828318166,3.78341131079859));
#16689=CARTESIAN_POINT('Ctrl Pts',(13.3204539021828,0.474232636092054,3.59008302369095));
#16690=CARTESIAN_POINT('Ctrl Pts',(13.3045486234952,0.305097944517489,3.48908297116948));
#16691=CARTESIAN_POINT('Ctrl Pts',(13.2886433448076,0.135963252942929,3.388082918648));
#16692=CARTESIAN_POINT('Ctrl Pts',(13.27273806612,-0.0883059379800925,3.3794111007127));
#16693=CARTESIAN_POINT('Ctrl Pts',(13.2568327874324,-0.264734703826722,
3.46704924928509));
#16694=CARTESIAN_POINT('Ctrl Pts',(13.2409275087448,-0.441163469673367,
3.55468739785749));
#16695=CARTESIAN_POINT('Ctrl Pts',(13.2250222300572,-0.569751810443623,
3.7386355129376));
#16696=CARTESIAN_POINT('Ctrl Pts',(13.2091169513696,-0.591457400179852,
3.9344324022836));
#16697=CARTESIAN_POINT('Ctrl Pts',(13.1932116726819,-0.613162989916079,
4.1302292916296));
#16698=CARTESIAN_POINT('Ctrl Pts',(13.1773063939943,-0.527985828618295,
4.33787495524147));
#16699=CARTESIAN_POINT('Ctrl Pts',(13.1614011153067,-0.375035665205916,
4.46202728915223));
#16700=CARTESIAN_POINT('Ctrl Pts',(13.150549213957,-0.270680367988337,4.54673431669939));
#16701=CARTESIAN_POINT('Ctrl Pts',(13.1396973126073,-0.134776053786733,
4.59257435599745));
#16702=CARTESIAN_POINT('Ctrl Pts',(13.1288454112576,0.000488576923893258,
4.59361798633976));
#16703=CARTESIAN_POINT('Ctrl Pts',(13.0211545887425,0.000215375668158819,
4.59498635240753));
#16704=CARTESIAN_POINT('Ctrl Pts',(13.0361060098081,-0.185045360160338,
4.59412349007018));
#16705=CARTESIAN_POINT('Ctrl Pts',(13.0510574308736,-0.371056311319581,
4.5007301079696));
#16706=CARTESIAN_POINT('Ctrl Pts',(13.0660088519392,-0.480360474535337,
4.35124746348123));
#16707=CARTESIAN_POINT('Ctrl Pts',(13.0819141306268,-0.596637928700896,
4.19222825660313));
#16708=CARTESIAN_POINT('Ctrl Pts',(13.0978194093145,-0.626109048224722,
3.96973483302036));
#16709=CARTESIAN_POINT('Ctrl Pts',(13.1137246880021,-0.555241941841719,
3.78592675992164));
#16710=CARTESIAN_POINT('Ctrl Pts',(13.1296299666897,-0.484374835458714,
3.60211868682292));
#16711=CARTESIAN_POINT('Ctrl Pts',(13.1455352453773,-0.313169503168878,
3.45699596420825));
#16712=CARTESIAN_POINT('Ctrl Pts',(13.1614405240649,-0.120236190459409,
3.4171928066662));
#16713=CARTESIAN_POINT('Ctrl Pts',(13.1773458027525,0.0726971222500488,
3.37738964912416));
#16714=CARTESIAN_POINT('Ctrl Pts',(13.1932510814401,0.287358415379145,3.44290605665475));
#16715=CARTESIAN_POINT('Ctrl Pts',(13.2091563601277,0.425184304693362,3.58365966669054));
#16716=CARTESIAN_POINT('Ctrl Pts',(13.2250616388154,0.563010194007583,3.72441327672633));
#16717=CARTESIAN_POINT('Ctrl Pts',(13.240966917503,0.624000679506934,3.94040408926733));
#16718=CARTESIAN_POINT('Ctrl Pts',(13.2568721961906,0.580151510544767,4.13245826101242));
#16719=CARTESIAN_POINT('Ctrl Pts',(13.2727774748782,0.536302341582597,4.32451243275751));
#16720=CARTESIAN_POINT('Ctrl Pts',(13.2886827535658,0.387613518158899,4.49262996370669));
#16721=CARTESIAN_POINT('Ctrl Pts',(13.3045880322534,0.202356657484476,4.55961839611428));
#16722=CARTESIAN_POINT('Ctrl Pts',(13.3101102177498,0.13803695776657,4.58287624384712));
#16723=CARTESIAN_POINT('Ctrl Pts',(13.3156324032461,0.0693092633201986,
4.59394375907155));
#16724=CARTESIAN_POINT('Ctrl Pts',(13.3211545887425,0.000436239896754628,
4.59347700091179));
#16725=CARTESIAN_POINT('Origin',(4.,0.,4.));
#16726=CARTESIAN_POINT('',(13.7288454112576,-0.000361622974213827,4.59480268714608));
#16727=CARTESIAN_POINT('',(13.6211545887425,-0.000396530615921017,4.59339874939382));
#16728=CARTESIAN_POINT('',(4.,-7.27562663373442E-17,4.5941));
#16729=CARTESIAN_POINT('Ctrl Pts',(13.7288454112576,-0.000361622974213827,
4.59480268714608));
#16730=CARTESIAN_POINT('Ctrl Pts',(13.714655378171,0.175608319374377,4.59354294412002));
#16731=CARTESIAN_POINT('Ctrl Pts',(13.7004653450845,0.352610168065205,4.51056419690263));
#16732=CARTESIAN_POINT('Ctrl Pts',(13.6862753119979,0.463013835099274,4.37381700684221));
#16733=CARTESIAN_POINT('Ctrl Pts',(13.6703700333103,0.586762742631886,4.22054025587244));
#16734=CARTESIAN_POINT('Ctrl Pts',(13.6544647546227,0.626840040937572,3.99971072753873));
#16735=CARTESIAN_POINT('Ctrl Pts',(13.6385594759351,0.564843930165024,3.81272399872504));
#16736=CARTESIAN_POINT('Ctrl Pts',(13.6226541972475,0.502847819392478,3.62573726991136));
#16737=CARTESIAN_POINT('Ctrl Pts',(13.6067489185599,0.338778299541704,3.4725933406177));
#16738=CARTESIAN_POINT('Ctrl Pts',(13.5908436398723,0.147969152919217,3.42360942419035));
#16739=CARTESIAN_POINT('Ctrl Pts',(13.5749383611846,-0.0428399937032757,
3.37462550776301));
#16740=CARTESIAN_POINT('Ctrl Pts',(13.559033082497,-0.260388767097474,3.42980160420198));
#16741=CARTESIAN_POINT('Ctrl Pts',(13.5431278038094,-0.404787974250376,
3.56380318433064));
#16742=CARTESIAN_POINT('Ctrl Pts',(13.5272225251218,-0.549187181403275,
3.6978047644593));
#16743=CARTESIAN_POINT('Ctrl Pts',(13.5113172464342,-0.620436822314871,
3.91063182827765));
#16744=CARTESIAN_POINT('Ctrl Pts',(13.4954119677466,-0.585822076202281,
4.10456319205082));
#16745=CARTESIAN_POINT('Ctrl Pts',(13.479506689059,-0.551207330089691,4.298494555824));
#16746=CARTESIAN_POINT('Ctrl Pts',(13.4636014103714,-0.410728196952908,
4.47353021955202));
#16747=CARTESIAN_POINT('Ctrl Pts',(13.4476961316837,-0.228886751546343,
4.54930121159921));
#16748=CARTESIAN_POINT('Ctrl Pts',(13.4414125582084,-0.15704808052867,4.57923546205676));
#16749=CARTESIAN_POINT('Ctrl Pts',(13.435128984733,-0.0787538239969463,
4.5936770685736));
#16750=CARTESIAN_POINT('Ctrl Pts',(13.4288454112576,-0.000323145728561625,
4.59329116515504));
#16751=CARTESIAN_POINT('Ctrl Pts',(13.3211545887425,0.000436239896754628,
4.59347700091179));
#16752=CARTESIAN_POINT('Ctrl Pts',(13.3315376819337,-0.129062311182503,
4.59259937855127));
#16753=CARTESIAN_POINT('Ctrl Pts',(13.341920775125,-0.259074650003773,4.55094414667863));
#16754=CARTESIAN_POINT('Ctrl Pts',(13.3523038683163,-0.361265427801182,
4.47287234722855));
#16755=CARTESIAN_POINT('Ctrl Pts',(13.3682091470039,-0.517805754487323,
4.35327853206923));
#16756=CARTESIAN_POINT('Ctrl Pts',(13.3841144256915,-0.609061509934468,
4.14823156788458));
#16757=CARTESIAN_POINT('Ctrl Pts',(13.4000197043791,-0.593131911953917,
3.95188034580653));
#16758=CARTESIAN_POINT('Ctrl Pts',(13.4159249830667,-0.577202313973367,
3.75552912372848));
#16759=CARTESIAN_POINT('Ctrl Pts',(13.4318302617543,-0.454087362565127,
3.56787364375704));
#16760=CARTESIAN_POINT('Ctrl Pts',(13.4477355404419,-0.280316234851803,
3.47507736324643));
#16761=CARTESIAN_POINT('Ctrl Pts',(13.4636408191295,-0.106545107138479,
3.38228108273583));
#16762=CARTESIAN_POINT('Ctrl Pts',(13.4795460978172,0.117882196879929,3.38434400168606));
#16763=CARTESIAN_POINT('Ctrl Pts',(13.4954513765048,0.2899181539344,3.48031891499009));
#16764=CARTESIAN_POINT('Ctrl Pts',(13.5113566551924,0.461954110988876,3.57629382829412));
#16765=CARTESIAN_POINT('Ctrl Pts',(13.52726193388,0.581598721079409,3.76618073595195));
#16766=CARTESIAN_POINT('Ctrl Pts',(13.5431672125676,0.593916240998451,3.96279160341967));
#16767=CARTESIAN_POINT('Ctrl Pts',(13.5590724912552,0.606233760917493,4.15940247088739));
#16768=CARTESIAN_POINT('Ctrl Pts',(13.5749777699428,0.511224190665043,4.362737298165));
#16769=CARTESIAN_POINT('Ctrl Pts',(13.5908830486304,0.352511905377589,4.47943333495374));
#16770=CARTESIAN_POINT('Ctrl Pts',(13.6009735620011,0.251822790258117,4.55346680161908));
#16771=CARTESIAN_POINT('Ctrl Pts',(13.6110640753718,0.125494626822297,4.59262991567553));
#16772=CARTESIAN_POINT('Ctrl Pts',(13.6211545887425,-0.000396530615921017,
4.59339874939382));
#16773=CARTESIAN_POINT('Origin',(4.,0.,4.));
#16774=CARTESIAN_POINT('',(14.0288454112576,0.000507412974116619,4.59441995931617));
#16775=CARTESIAN_POINT('',(13.9211545887425,-0.000275297881949146,4.59492513410986));
#16776=CARTESIAN_POINT('',(4.,-7.27562663373442E-17,4.5941));
#16777=CARTESIAN_POINT('Ctrl Pts',(14.0288454112576,0.000507412974116619,
4.59441995931617));
#16778=CARTESIAN_POINT('Ctrl Pts',(14.0259923289843,0.0359476882196221,
4.59474138052009));
#16779=CARTESIAN_POINT('Ctrl Pts',(14.0231392467111,0.0713355155074759,
4.59184535342408));
#16780=CARTESIAN_POINT('Ctrl Pts',(14.0202861644378,0.106106362061302,4.58554453803953));
#16781=CARTESIAN_POINT('Ctrl Pts',(14.0043808857502,0.299945849210873,4.55041893875697));
#16782=CARTESIAN_POINT('Ctrl Pts',(13.9884756070626,0.474610768799237,4.40947910659883));
#16783=CARTESIAN_POINT('Ctrl Pts',(13.972570328375,0.549902379214768,4.22743864981956));
#16784=CARTESIAN_POINT('Ctrl Pts',(13.9566650496873,0.625193989630293,4.04539819304031));
#16785=CARTESIAN_POINT('Ctrl Pts',(13.9407597709997,0.601112290873006,3.82225711163994));
#16786=CARTESIAN_POINT('Ctrl Pts',(13.9248544923121,0.488714580199595,3.66047234987686));
#16787=CARTESIAN_POINT('Ctrl Pts',(13.9089492136245,0.376316869526181,3.49868758811377));
#16788=CARTESIAN_POINT('Ctrl Pts',(13.8930439349369,0.175603146936639,3.39825914598798));
#16789=CARTESIAN_POINT('Ctrl Pts',(13.8771386562493,-0.0212673376532481,
3.40529951534663));
#16790=CARTESIAN_POINT('Ctrl Pts',(13.8612333775617,-0.218137822243141,
3.41233988470529));
#16791=CARTESIAN_POINT('Ctrl Pts',(13.8453280988741,-0.411165068833379,
3.52684906554841));
#16792=CARTESIAN_POINT('Ctrl Pts',(13.8294228201864,-0.511719132099071,
3.69624928651676));
#16793=CARTESIAN_POINT('Ctrl Pts',(13.8135175414988,-0.612273195364761,
3.8656495074851));
#16794=CARTESIAN_POINT('Ctrl Pts',(13.7976122628112,-0.62035407530591,4.08994076857866));
#16795=CARTESIAN_POINT('Ctrl Pts',(13.7817069841236,-0.532251373727382,
4.26613801168402));
#16796=CARTESIAN_POINT('Ctrl Pts',(13.765801705436,-0.44414867214885,4.44233525478938));
#16797=CARTESIAN_POINT('Ctrl Pts',(13.7498964267484,-0.259862389050636,
4.57043847990653));
#16798=CARTESIAN_POINT('Ctrl Pts',(13.7339911480608,-0.0640089891217576,
4.59162810566218));
#16799=CARTESIAN_POINT('Ctrl Pts',(13.7322759024597,-0.0428879079209441,
4.59391322201126));
#16800=CARTESIAN_POINT('Ctrl Pts',(13.7305606568586,-0.0216323041412813,
4.594954960835));
#16801=CARTESIAN_POINT('Ctrl Pts',(13.7288454112576,-0.000361622974213827,
4.59480268714608));
#16802=CARTESIAN_POINT('Ctrl Pts',(13.6211545887425,-0.000396530615921017,
4.59339874939382));
#16803=CARTESIAN_POINT('Ctrl Pts',(13.6269693540594,-0.0729426448807452,
4.59384179797573));
#16804=CARTESIAN_POINT('Ctrl Pts',(13.6327841193764,-0.145343639818557,
4.58153501668255));
#16805=CARTESIAN_POINT('Ctrl Pts',(13.6385988846933,-0.212609537044371,
4.5558040579697));
#16806=CARTESIAN_POINT('Ctrl Pts',(13.6545041633809,-0.396603693856438,
4.48542149789704));
#16807=CARTESIAN_POINT('Ctrl Pts',(13.6704094420685,-0.542177007158105,
4.31459913145184));
#16808=CARTESIAN_POINT('Ctrl Pts',(13.6863147207561,-0.582488370180261,
4.12177136240739));
#16809=CARTESIAN_POINT('Ctrl Pts',(13.7022199994437,-0.622799733202417,
3.92894359336294));
#16810=CARTESIAN_POINT('Ctrl Pts',(13.7181252781313,-0.557849145945042,
3.71411042171923));
#16811=CARTESIAN_POINT('Ctrl Pts',(13.734030556819,-0.417459170243993,3.57591415105311));
#16812=CARTESIAN_POINT('Ctrl Pts',(13.7499358355066,-0.277069194542941,
3.43771788038699));
#16813=CARTESIAN_POINT('Ctrl Pts',(13.7658411141942,-0.0612398303982075,
3.37615851069845));
#16814=CARTESIAN_POINT('Ctrl Pts',(13.7817463928818,0.130929209162332,3.41950150018632));
#16815=CARTESIAN_POINT('Ctrl Pts',(13.7976516715694,0.323098248722867,3.46284448967418));
#16816=CARTESIAN_POINT('Ctrl Pts',(13.813556950257,0.491606963699209,3.61108983833845));
#16817=CARTESIAN_POINT('Ctrl Pts',(13.8294622289446,0.559083281190044,3.79616955381596));
#16818=CARTESIAN_POINT('Ctrl Pts',(13.8453675076322,0.62655959868088,3.98124926929349));
#16819=CARTESIAN_POINT('Ctrl Pts',(13.8612727863198,0.593003518686204,4.20316335158427));
#16820=CARTESIAN_POINT('Ctrl Pts',(13.8771780650075,0.4738225734989,4.36001824251097));
#16821=CARTESIAN_POINT('Ctrl Pts',(13.8918369062525,0.363981395029584,4.50458099992985));
#16822=CARTESIAN_POINT('Ctrl Pts',(13.9064957474975,0.181409709145346,4.59388191268165));
#16823=CARTESIAN_POINT('Ctrl Pts',(13.9211545887425,-0.000275297881949146,
4.59492513410986));
#16824=CARTESIAN_POINT('Origin',(4.,0.,4.));
#16825=CARTESIAN_POINT('',(14.3288454112576,0.000109044058801022,4.5931342436645));
#16826=CARTESIAN_POINT('',(14.2211545887425,0.000537210645871958,4.59424369460725));
#16827=CARTESIAN_POINT('',(4.,-7.27562663373442E-17,4.5941));
#16828=CARTESIAN_POINT('Ctrl Pts',(14.3288454112576,0.000109044058801022,
4.5931342436645));
#16829=CARTESIAN_POINT('Ctrl Pts',(14.32142400111,0.0928032711674493,4.59328573107644));
#16830=CARTESIAN_POINT('Ctrl Pts',(14.3140025909624,0.185434358886594,4.57287353691408));
#16831=CARTESIAN_POINT('Ctrl Pts',(14.3065811808148,0.267539471941071,4.53154830171049));
#16832=CARTESIAN_POINT('Ctrl Pts',(14.2906759021272,0.443503969097433,4.44298165875801));
#16833=CARTESIAN_POINT('Ctrl Pts',(14.2747706234396,0.571121189235106,4.25835848700565));
#16834=CARTESIAN_POINT('Ctrl Pts',(14.258865344752,0.591794703906212,4.06244993615984));
#16835=CARTESIAN_POINT('Ctrl Pts',(14.2429600660644,0.612468218577319,3.86654138531401));
#16836=CARTESIAN_POINT('Ctrl Pts',(14.2270547873768,0.526198027781844,3.65934745537473));
#16837=CARTESIAN_POINT('Ctrl Pts',(14.2111495086891,0.372595753342289,3.53600283331781));
#16838=CARTESIAN_POINT('Ctrl Pts',(14.1952442300015,0.218993478902743,3.4126582112609));
#16839=CARTESIAN_POINT('Ctrl Pts',(14.1793389513139,-0.00194087918087354,
3.37316289708635));
#16840=CARTESIAN_POINT('Ctrl Pts',(14.1634336726263,-0.18876361063844,3.43565146815417));
#16841=CARTESIAN_POINT('Ctrl Pts',(14.1475283939387,-0.375586342096006,
3.49814003922198));
#16842=CARTESIAN_POINT('Ctrl Pts',(14.1316231152511,-0.528297446927522,
3.66261249553216));
#16843=CARTESIAN_POINT('Ctrl Pts',(14.1157178365635,-0.576778446468407,
3.85355004340287));
#16844=CARTESIAN_POINT('Ctrl Pts',(14.0998125578759,-0.625259446009293,
4.04448759127359));
#16845=CARTESIAN_POINT('Ctrl Pts',(14.0839072791882,-0.569510340259543,
4.26189023070484));
#16846=CARTESIAN_POINT('Ctrl Pts',(14.0680020005006,-0.435128760029281,
4.40593586721696));
#16847=CARTESIAN_POINT('Ctrl Pts',(14.0549498040863,-0.324852491748397,
4.52414265738481));
#16848=CARTESIAN_POINT('Ctrl Pts',(14.0418976076719,-0.161623710204441,
4.5929495310973));
#16849=CARTESIAN_POINT('Ctrl Pts',(14.0288454112576,0.000507412974116619,
4.59441995931617));
#16850=CARTESIAN_POINT('Ctrl Pts',(13.9211545887425,-0.000275297881949146,
4.59492513410986));
#16851=CARTESIAN_POINT('Ctrl Pts',(13.9224010261851,-0.015723926578741,
4.59501383895544));
#16852=CARTESIAN_POINT('Ctrl Pts',(13.9236474636277,-0.0311661445373128,
4.59446443570748));
#16853=CARTESIAN_POINT('Ctrl Pts',(13.9248939010703,-0.0465566941337027,
4.59325663951544));
#16854=CARTESIAN_POINT('Ctrl Pts',(13.9407991797579,-0.242949206199084,
4.5778444460306));
#16855=CARTESIAN_POINT('Ctrl Pts',(13.9567044584455,-0.430928419949921,
4.4552243594983));
#16856=CARTESIAN_POINT('Ctrl Pts',(13.9726097371331,-0.524182233176515,
4.28169833602613));
#16857=CARTESIAN_POINT('Ctrl Pts',(13.9885150158207,-0.617436046403107,
4.10817231255396));
#16858=CARTESIAN_POINT('Ctrl Pts',(14.0044202945084,-0.615964459105464,
3.88374035214192));
#16859=CARTESIAN_POINT('Ctrl Pts',(14.020325573196,-0.52044316191294,3.71145211607799));
#16860=CARTESIAN_POINT('Ctrl Pts',(14.0362308518836,-0.424921864720413,
3.53916388001405));
#16861=CARTESIAN_POINT('Ctrl Pts',(14.0521361305712,-0.235350857633014,
3.41901936829824));
#16862=CARTESIAN_POINT('Ctrl Pts',(14.0680414092588,-0.0387731270173405,
3.40618385781531));
#16863=CARTESIAN_POINT('Ctrl Pts',(14.0839466879464,0.157804603598333,3.39334834733239));
#16864=CARTESIAN_POINT('Ctrl Pts',(14.0998519666341,0.361389057742269,3.48782183808236));
#16865=CARTESIAN_POINT('Ctrl Pts',(14.1157572453217,0.478502867019537,3.64622609995664));
#16866=CARTESIAN_POINT('Ctrl Pts',(14.1316625240093,0.595616676296804,3.80463036183091));
#16867=CARTESIAN_POINT('Ctrl Pts',(14.1475678026969,0.626259840707404,4.02696539482948));
#16868=CARTESIAN_POINT('Ctrl Pts',(14.1634730813845,0.556362315559365,4.21114435801894));
#16869=CARTESIAN_POINT('Ctrl Pts',(14.1793783600721,0.486464790411328,4.3953233212084));
#16870=CARTESIAN_POINT('Ctrl Pts',(14.1952836387597,0.316026575704654,4.54134621458875));
#16871=CARTESIAN_POINT('Ctrl Pts',(14.2111889174473,0.123305688986428,4.58216550323889));
#16872=CARTESIAN_POINT('Ctrl Pts',(14.2145108078791,0.0830550475387342,
4.59069079896363));
#16873=CARTESIAN_POINT('Ctrl Pts',(14.2178326983108,0.0418324306113591,
4.59462708830176));
#16874=CARTESIAN_POINT('Ctrl Pts',(14.2211545887425,0.000537210645871958,
4.59424369460725));
#16875=CARTESIAN_POINT('Origin',(4.,0.,4.));
#16876=CARTESIAN_POINT('',(14.6288454112575,-0.000548182068839831,4.59401855345973));
#16877=CARTESIAN_POINT('',(14.5211545887425,1.28950532977596E-5,4.59311636453746));
#16878=CARTESIAN_POINT('',(4.,-7.27562663373442E-17,4.5941));
#16879=CARTESIAN_POINT('Ctrl Pts',(14.6288454112575,-0.000548182068839831,
4.59401855345973));
#16880=CARTESIAN_POINT('Ctrl Pts',(14.6168556732357,0.148643716013534,4.59265593252186));
#16881=CARTESIAN_POINT('Ctrl Pts',(14.6048659352138,0.29876355451001,4.53564313143304));
#16882=CARTESIAN_POINT('Ctrl Pts',(14.5928761971919,0.407080942069735,4.43405768361063));
#16883=CARTESIAN_POINT('Ctrl Pts',(14.5769709185042,0.55077200793829,4.29929703619113));
#16884=CARTESIAN_POINT('Ctrl Pts',(14.5610656398166,0.620899143473568,4.08609746938767));
#16885=CARTESIAN_POINT('Ctrl Pts',(14.545160361129,0.585262934872208,3.89235120454656));
#16886=CARTESIAN_POINT('Ctrl Pts',(14.5292550824414,0.549626726270847,3.69860493970543));
#16887=CARTESIAN_POINT('Ctrl Pts',(14.5133498037538,0.408227173532835,3.52431197682665));
#16888=CARTESIAN_POINT('Ctrl Pts',(14.4974445250662,0.225988969153725,3.44950027073699));
#16889=CARTESIAN_POINT('Ctrl Pts',(14.4815392463786,0.04375076477463,3.37468856464734));
#16890=CARTESIAN_POINT('Ctrl Pts',(14.465633967691,-0.179326091245555,3.39935811534679));
#16891=CARTESIAN_POINT('Ctrl Pts',(14.4497286890033,-0.340814144225853,
3.51218170883678));
#16892=CARTESIAN_POINT('Ctrl Pts',(14.4338234103157,-0.50230219720616,3.62500530232677));
#16893=CARTESIAN_POINT('Ctrl Pts',(14.4179181316281,-0.602201447146573,
3.82598293860731));
#16894=CARTESIAN_POINT('Ctrl Pts',(14.4020128529405,-0.594642384863179,
4.02283418976097));
#16895=CARTESIAN_POINT('Ctrl Pts',(14.3861075742529,-0.587083322579785,
4.21968544091462));
#16896=CARTESIAN_POINT('Ctrl Pts',(14.3702022955653,-0.47206594807259,4.4124103069414));
#16897=CARTESIAN_POINT('Ctrl Pts',(14.3542970168777,-0.302401373731467,
4.51251768287848));
#16898=CARTESIAN_POINT('Ctrl Pts',(14.3458131483376,-0.211902365642262,
4.565914912441));
#16899=CARTESIAN_POINT('Ctrl Pts',(14.3373292797976,-0.10585540495725,4.59296106912451));
#16900=CARTESIAN_POINT('Ctrl Pts',(14.3288454112576,0.000109044058801022,
4.5931342436645));
#16901=CARTESIAN_POINT('Ctrl Pts',(14.2211545887425,0.000537210645871958,
4.59424369460725));
#16902=CARTESIAN_POINT('Ctrl Pts',(14.2337379769984,-0.155889919212927,
4.59279139152499));
#16903=CARTESIAN_POINT('Ctrl Pts',(14.2463213652543,-0.313358837143528,
4.52935553548989));
#16904=CARTESIAN_POINT('Ctrl Pts',(14.2589047535102,-0.422984449084643,
4.4185751090669));
#16905=CARTESIAN_POINT('Ctrl Pts',(14.2748100321978,-0.561550141707708,
4.27854974232482));
#16906=CARTESIAN_POINT('Ctrl Pts',(14.2907153108854,-0.623677968224056,
4.06288332492072));
#16907=CARTESIAN_POINT('Ctrl Pts',(14.306620589573,-0.580841459108965,3.87060075163287));
#16908=CARTESIAN_POINT('Ctrl Pts',(14.3225258682606,-0.538004949993874,
3.67831817834502));
#16909=CARTESIAN_POINT('Ctrl Pts',(14.3384311469482,-0.390204105247342,
3.50941944917344));
#16910=CARTESIAN_POINT('Ctrl Pts',(14.3543364256359,-0.205302819838896,
3.44145571503774));
#16911=CARTESIAN_POINT('Ctrl Pts',(14.3702417043235,-0.0204015344304391,
3.37349198090203));
#16912=CARTESIAN_POINT('Ctrl Pts',(14.3861469830111,0.201600191639931,3.40646324180223));
#16913=CARTESIAN_POINT('Ctrl Pts',(14.4020522616987,0.358768557879186,3.52523048963197));
#16914=CARTESIAN_POINT('Ctrl Pts',(14.4179575403863,0.515936924118427,3.6439977374617));
#16915=CARTESIAN_POINT('Ctrl Pts',(14.4338628190739,0.608271930526566,3.84856097222098));
#16916=CARTESIAN_POINT('Ctrl Pts',(14.4497680977615,0.59337724853295,4.04499341086509));
#16917=CARTESIAN_POINT('Ctrl Pts',(14.4656733764491,0.578482566539332,4.2414258495092));
#16918=CARTESIAN_POINT('Ctrl Pts',(14.4815786551367,0.456358196143958,4.42972749203816));
#16919=CARTESIAN_POINT('Ctrl Pts',(14.4974839338244,0.283078481576349,4.52343819058819));
#16920=CARTESIAN_POINT('Ctrl Pts',(14.5053741521304,0.197118668938093,4.56992576768087));
#16921=CARTESIAN_POINT('Ctrl Pts',(14.5132643704364,0.0985699939877532,
4.59313537862966));
#16922=CARTESIAN_POINT('Ctrl Pts',(14.5211545887425,1.28950532977596E-5,
4.59311636453746));
#16923=CARTESIAN_POINT('Origin',(4.,0.,4.));
#16924=CARTESIAN_POINT('',(14.9288454112575,0.000149915246051877,4.59503491979621));
#16925=CARTESIAN_POINT('',(14.8211545887425,-0.000542004001680995,4.59419620878869));
#16926=CARTESIAN_POINT('',(4.,-7.27562663373442E-17,4.5941));
#16927=CARTESIAN_POINT('Ctrl Pts',(14.9288454112575,0.000149915246051877,
4.59503491979621));
#16928=CARTESIAN_POINT('Ctrl Pts',(14.9281926240489,0.00823674021970066,
4.59506221957623));
#16929=CARTESIAN_POINT('Ctrl Pts',(14.9275398368403,0.0163225255999611,
4.59491168338633));
#16930=CARTESIAN_POINT('Ctrl Pts',(14.9268870496317,0.0244008833477238,
4.59458015690877));
#16931=CARTESIAN_POINT('Ctrl Pts',(14.9109817709441,0.221231534471853,4.58650245417764));
#16932=CARTESIAN_POINT('Ctrl Pts',(14.8950764922565,0.413652681988333,4.47097768448731));
#16933=CARTESIAN_POINT('Ctrl Pts',(14.8791712135689,0.513312675625014,4.30104993462962));
#16934=CARTESIAN_POINT('Ctrl Pts',(14.8632659348813,0.612972669261697,4.13112218477192));
#16935=CARTESIAN_POINT('Ctrl Pts',(14.8473606561937,0.619871509018575,3.90679145474687));
#16936=CARTESIAN_POINT('Ctrl Pts',(14.831455377506,0.530841539545133,3.73106092513143));
#16937=CARTESIAN_POINT('Ctrl Pts',(14.8155500988184,0.441811570071688,3.55533039551599));
#16938=CARTESIAN_POINT('Ctrl Pts',(14.7996448201308,0.256852791367914,3.42820006631018));
#16939=CARTESIAN_POINT('Ctrl Pts',(14.7837395414432,0.0608904496539635,
3.40804280624462));
#16940=CARTESIAN_POINT('Ctrl Pts',(14.7678342627556,-0.135071892059981,
3.38788554617906));
#16941=CARTESIAN_POINT('Ctrl Pts',(14.751928984068,-0.342037796784102,3.47470135525375));
#16942=CARTESIAN_POINT('Ctrl Pts',(14.7360237053804,-0.464977277074429,
3.62862808681558));
#16943=CARTESIAN_POINT('Ctrl Pts',(14.7201184266927,-0.587916757364756,
3.78255481837741));
#16944=CARTESIAN_POINT('Ctrl Pts',(14.7042131480052,-0.62682981322129,4.00359247242638));
#16945=CARTESIAN_POINT('Ctrl Pts',(14.6883078693175,-0.56384921567034,4.19024990955517));
#16946=CARTESIAN_POINT('Ctrl Pts',(14.6724025906299,-0.500868618119389,
4.37690734668397));
#16947=CARTESIAN_POINT('Ctrl Pts',(14.6564973119423,-0.335994367160947,
4.52918456689258));
#16948=CARTESIAN_POINT('Ctrl Pts',(14.6405920332547,-0.144929743580805,
4.57716231297912));
#16949=CARTESIAN_POINT('Ctrl Pts',(14.636676492589,-0.097893704910838,4.5889734116427));
#16950=CARTESIAN_POINT('Ctrl Pts',(14.6327609519233,-0.0492704262804658,
4.59446355048005));
#16951=CARTESIAN_POINT('Ctrl Pts',(14.6288454112575,-0.000548182068839831,
4.59401855345973));
#16952=CARTESIAN_POINT('Ctrl Pts',(14.5211545887425,1.28950532977596E-5,
4.59311636453746));
#16953=CARTESIAN_POINT('Ctrl Pts',(14.5291696491241,-0.100103612291989,
4.59309704959697));
#16954=CARTESIAN_POINT('Ctrl Pts',(14.5371847095056,-0.200228812305367,
4.56910822985942));
#16955=CARTESIAN_POINT('Ctrl Pts',(14.5451997698872,-0.287175610734119,
4.52120162576233));
#16956=CARTESIAN_POINT('Ctrl Pts',(14.5611050485748,-0.459714929737158,
4.42613460781534));
#16957=CARTESIAN_POINT('Ctrl Pts',(14.5770103272624,-0.580358509003398,
4.23688081735026));
#16958=CARTESIAN_POINT('Ctrl Pts',(14.59291560595,-0.593711920942704,4.04033758828107));
#16959=CARTESIAN_POINT('Ctrl Pts',(14.6088208846377,-0.607065332882009,
3.84379435921188));
#16960=CARTESIAN_POINT('Ctrl Pts',(14.6247261633253,-0.513128577494387,
3.63996169153858));
#16961=CARTESIAN_POINT('Ctrl Pts',(14.6406314420129,-0.35503343871745,3.52243092280774));
#16962=CARTESIAN_POINT('Ctrl Pts',(14.6565367207005,-0.196938299940509,
3.40490015407689));
#16963=CARTESIAN_POINT('Ctrl Pts',(14.6724419993881,0.025315222225754,3.37367128428849));
#16964=CARTESIAN_POINT('Ctrl Pts',(14.6883472780757,0.209677713173688,3.44308328926485));
#16965=CARTESIAN_POINT('Ctrl Pts',(14.7042525567633,0.394040204121622,3.51249529424121));
#16966=CARTESIAN_POINT('Ctrl Pts',(14.720157835451,0.540511663851219,3.68254817398232));
#16967=CARTESIAN_POINT('Ctrl Pts',(14.7360631141386,0.581838594751101,3.87516084045512));
#16968=CARTESIAN_POINT('Ctrl Pts',(14.7519683928262,0.623165525650983,4.06777350692792));
#16969=CARTESIAN_POINT('Ctrl Pts',(14.7678736715138,0.559347927721136,4.2829459601324));
#16970=CARTESIAN_POINT('Ctrl Pts',(14.7837789502014,0.419688142031033,4.42188011275284));
#16971=CARTESIAN_POINT('Ctrl Pts',(14.7962374963817,0.310293146587505,4.53070672248707));
#16972=CARTESIAN_POINT('Ctrl Pts',(14.8086960425621,0.154364940471616,4.59275708529138));
#16973=CARTESIAN_POINT('Ctrl Pts',(14.8211545887425,-0.000542004001680995,
4.59419620878869));
#16974=CARTESIAN_POINT('Origin',(4.,0.,4.));
#16975=CARTESIAN_POINT('',(15.2288454112576,0.000471544078774977,4.59356550157774));
#16976=CARTESIAN_POINT('',(15.1211545887425,0.000250233060073018,4.59495282954609));
#16977=CARTESIAN_POINT('',(4.,-7.27562663373442E-17,4.5941));
#16978=CARTESIAN_POINT('Ctrl Pts',(15.2288454112576,0.000471544078774977,
4.59356550157774));
#16979=CARTESIAN_POINT('Ctrl Pts',(15.2236242961746,0.0655651715058866,
4.59404721416646));
#16980=CARTESIAN_POINT('Ctrl Pts',(15.2184031810917,0.130516835945995,4.58418155789741));
#16981=CARTESIAN_POINT('Ctrl Pts',(15.2131820660088,0.191734887706884,4.56334598510492));
#16982=CARTESIAN_POINT('Ctrl Pts',(15.1972767873211,0.378225734681762,4.49987379829874));
#16983=CARTESIAN_POINT('Ctrl Pts',(15.1813715086335,0.530068013118856,4.33459889729257));
#16984=CARTESIAN_POINT('Ctrl Pts',(15.1654662299459,0.577542172676889,4.143408524424));
#16985=CARTESIAN_POINT('Ctrl Pts',(15.1495609512583,0.625016332234921,3.95221815155542));
#16986=CARTESIAN_POINT('Ctrl Pts',(15.1336556725707,0.568122372913892,3.73511230682445));
#16987=CARTESIAN_POINT('Ctrl Pts',(15.1177503938831,0.432983593849097,3.59177680914072));
#16988=CARTESIAN_POINT('Ctrl Pts',(15.1018451151955,0.297844814784303,3.44844131145699));
#16989=CARTESIAN_POINT('Ctrl Pts',(15.0859398365078,0.0844612159757424,
3.37887616082051));
#16990=CARTESIAN_POINT('Ctrl Pts',(15.0700345578202,-0.109190481519281,
3.41502273134472));
#16991=CARTESIAN_POINT('Ctrl Pts',(15.0541292791326,-0.302842179014298,
3.45116930186893));
#16992=CARTESIAN_POINT('Ctrl Pts',(15.038224000445,-0.47676197519578,3.59302759355383));
#16993=CARTESIAN_POINT('Ctrl Pts',(15.0223187217574,-0.551093257596978,
3.77546228038711));
#16994=CARTESIAN_POINT('Ctrl Pts',(15.0064134430698,-0.625424539998176,
3.95789696722038));
#16995=CARTESIAN_POINT('Ctrl Pts',(14.9905081643822,-0.600167308619091,
4.18090804920204));
#16996=CARTESIAN_POINT('Ctrl Pts',(14.9746028856946,-0.486918615563658,
4.34209827230691));
#16997=CARTESIAN_POINT('Ctrl Pts',(14.9593503942156,-0.378317895025423,
4.49667289829699));
#16998=CARTESIAN_POINT('Ctrl Pts',(14.9440979027365,-0.188800216398263,
4.59439705548643));
#16999=CARTESIAN_POINT('Ctrl Pts',(14.9288454112575,0.000149915246051877,
4.59503491979621));
#17000=CARTESIAN_POINT('Ctrl Pts',(14.8211545887425,-0.000542004001680995,
4.59419620878869));
#17001=CARTESIAN_POINT('Ctrl Pts',(14.8246013212497,-0.0433979515083632,
4.5945943510493));
#17002=CARTESIAN_POINT('Ctrl Pts',(14.828048053757,-0.0861757330942537,
4.59035339483295));
#17003=CARTESIAN_POINT('Ctrl Pts',(14.8314947862642,-0.127868389248254,
4.58118038604969));
#17004=CARTESIAN_POINT('Ctrl Pts',(14.8474000649518,-0.320263161387096,
4.5388506546897));
#17005=CARTESIAN_POINT('Ctrl Pts',(14.8633053436395,-0.489550732214419,
4.39149533993331));
#17006=CARTESIAN_POINT('Ctrl Pts',(14.8792106223271,-0.558001411172811,
4.20677376822741));
#17007=CARTESIAN_POINT('Ctrl Pts',(14.8951159010147,-0.6264520901312,4.0220521965215));
#17008=CARTESIAN_POINT('Ctrl Pts',(14.9110211797023,-0.594065877220663,
3.79996436786608));
#17009=CARTESIAN_POINT('Ctrl Pts',(14.9269264583899,-0.475713151262041,
3.64248361741852));
#17010=CARTESIAN_POINT('Ctrl Pts',(14.9428317370775,-0.357360425303418,
3.48500286697096));
#17011=CARTESIAN_POINT('Ctrl Pts',(14.9587370157651,-0.153041186296697,
3.39212919473125));
#17012=CARTESIAN_POINT('Ctrl Pts',(14.9746422944528,0.0434298152403689,
3.40650626183085));
#17013=CARTESIAN_POINT('Ctrl Pts',(14.9905475731404,0.239900816777435,3.42088332893044));
#17014=CARTESIAN_POINT('Ctrl Pts',(15.006452851828,0.428523580844854,3.54251113536931));
#17015=CARTESIAN_POINT('Ctrl Pts',(15.0223581305156,0.522690514153935,3.71554333807889));
#17016=CARTESIAN_POINT('Ctrl Pts',(15.0382634092032,0.616857447463019,3.88857554078846));
#17017=CARTESIAN_POINT('Ctrl Pts',(15.0541686878908,0.616568550013756,4.11301213976874));
#17018=CARTESIAN_POINT('Ctrl Pts',(15.0700739665784,0.521956471292605,4.28580134389743));
#17019=CARTESIAN_POINT('Ctrl Pts',(15.085979245266,0.427344392571456,4.45859054802613));
#17020=CARTESIAN_POINT('Ctrl Pts',(15.1018845239536,0.238409132578427,4.57973235730324));
#17021=CARTESIAN_POINT('Ctrl Pts',(15.1177898026413,0.0419017695106382,
4.59360357799603));
#17022=CARTESIAN_POINT('Ctrl Pts',(15.1189113980083,0.0280446248267054,
4.59458173733358));
#17023=CARTESIAN_POINT('Ctrl Pts',(15.1200329933754,0.0141498265549413,
4.59502647517791));
#17024=CARTESIAN_POINT('Ctrl Pts',(15.1211545887425,0.000250233060073018,
4.59495282954609));
#17025=CARTESIAN_POINT('Origin',(4.,0.,4.));
#17026=CARTESIAN_POINT('',(15.5288454112575,-0.000350670266729247,4.59332700645389));
#17027=CARTESIAN_POINT('',(15.4211545887425,0.000414092275955974,4.59343115273787));
#17028=CARTESIAN_POINT('',(4.,-7.27562663373442E-17,4.5941));
#17029=CARTESIAN_POINT('Ctrl Pts',(15.5288454112575,-0.000350670266729247,
4.59332700645389));
#17030=CARTESIAN_POINT('Ctrl Pts',(15.5190559683003,0.121821298278883,4.59267222728074));
#17031=CARTESIAN_POINT('Ctrl Pts',(15.509266525343,0.244354036528086,4.55597946496206));
#17032=CARTESIAN_POINT('Ctrl Pts',(15.4994770823858,0.343380025451582,4.48601555964668));
#17033=CARTESIAN_POINT('Ctrl Pts',(15.4835718036982,0.504271299656008,4.37234255322809));
#17034=CARTESIAN_POINT('Ctrl Pts',(15.4676665250105,0.603110088323456,4.17084127710728));
#17035=CARTESIAN_POINT('Ctrl Pts',(15.4517612463229,0.594513801222153,3.97403259246294));
#17036=CARTESIAN_POINT('Ctrl Pts',(15.4358559676353,0.58591751412085,3.7772239078186));
#17037=CARTESIAN_POINT('Ctrl Pts',(15.4199506889477,0.469886151250777,3.58510781465072));
#17038=CARTESIAN_POINT('Ctrl Pts',(15.4040454102601,0.299696405559752,3.48589589518039));
#17039=CARTESIAN_POINT('Ctrl Pts',(15.3881401315725,0.129506659868722,3.38668397571006));
#17040=CARTESIAN_POINT('Ctrl Pts',(15.3722348528849,-0.0948414686432761,
3.38037622993726));
#17041=CARTESIAN_POINT('Ctrl Pts',(15.3563295741973,-0.270336810750117,
3.46986890786216));
#17042=CARTESIAN_POINT('Ctrl Pts',(15.3404242955096,-0.445832152856957,
3.55936158578705));
#17043=CARTESIAN_POINT('Ctrl Pts',(15.324519016822,-0.572474708558633,3.74465468740961));
#17044=CARTESIAN_POINT('Ctrl Pts',(15.3086137381344,-0.592115574081638,
3.94066945956945));
#17045=CARTESIAN_POINT('Ctrl Pts',(15.2927084594468,-0.611756439604643,
4.13668423172929));
#17046=CARTESIAN_POINT('Ctrl Pts',(15.2768031807592,-0.524395614948954,
4.3434206744264));
#17047=CARTESIAN_POINT('Ctrl Pts',(15.2608979020716,-0.370145494864779,
4.46595415947185));
#17048=CARTESIAN_POINT('Ctrl Pts',(15.2502137384669,-0.266529987624151,
4.54826443060822));
#17049=CARTESIAN_POINT('Ctrl Pts',(15.2395295748622,-0.13273198696893,4.59257975504152));
#17050=CARTESIAN_POINT('Ctrl Pts',(15.2288454112576,0.000471544078774977,
4.59356550157774));
#17051=CARTESIAN_POINT('Ctrl Pts',(15.1211545887425,0.000250233060073018,
4.59495282954609));
#17052=CARTESIAN_POINT('Ctrl Pts',(15.135938272063,-0.18295950063263,4.59398211075496));
#17053=CARTESIAN_POINT('Ctrl Pts',(15.1507219553836,-0.367002343096231,
4.50294888365168));
#17054=CARTESIAN_POINT('Ctrl Pts',(15.1655056387041,-0.476631971954554,
4.35629051265579));
#17055=CARTESIAN_POINT('Ctrl Pts',(15.1814109173917,-0.594578884209397,
4.19850559451431));
#17056=CARTESIAN_POINT('Ctrl Pts',(15.1973161960793,-0.626393242576541,
3.97633512612291));
#17057=CARTESIAN_POINT('Ctrl Pts',(15.2132214747669,-0.557467239648298,
3.79179038730953));
#17058=CARTESIAN_POINT('Ctrl Pts',(15.2291267534545,-0.488541236720055,
3.60724564849615));
#17059=CARTESIAN_POINT('Ctrl Pts',(15.2450320321422,-0.318874872496425,
3.46032663926078));
#17060=CARTESIAN_POINT('Ctrl Pts',(15.2609373108298,-0.126371763436977,
3.41849235301362));
#17061=CARTESIAN_POINT('Ctrl Pts',(15.2768425895174,0.0661313456224706,
3.37665806676646));
#17062=CARTESIAN_POINT('Ctrl Pts',(15.292747868205,0.281471199517752,3.4399085035075));
#17063=CARTESIAN_POINT('Ctrl Pts',(15.3086531468926,0.420772847618048,3.57920173859056));
#17064=CARTESIAN_POINT('Ctrl Pts',(15.3245584255802,0.560074495718348,3.71849497367363));
#17065=CARTESIAN_POINT('Ctrl Pts',(15.3404637042678,0.623337938023671,3.9338310070987));
#17066=CARTESIAN_POINT('Ctrl Pts',(15.3563689829554,0.581515278282945,4.12633664243329));
#17067=CARTESIAN_POINT('Ctrl Pts',(15.3722742616431,0.53969261854222,4.31884227776789));
#17068=CARTESIAN_POINT('Ctrl Pts',(15.3881795403307,0.392783856755445,4.48851751501199));
#17069=CARTESIAN_POINT('Ctrl Pts',(15.4040848190183,0.208243281137944,4.55745466359042));
#17070=CARTESIAN_POINT('Ctrl Pts',(15.4097747422597,0.142226097106806,4.58211610408423));
#17071=CARTESIAN_POINT('Ctrl Pts',(15.4154646655011,0.0713929250243718,
4.593885435962));
#17072=CARTESIAN_POINT('Ctrl Pts',(15.4211545887425,0.000414092275955974,
4.59343115273787));
#17073=CARTESIAN_POINT('Origin',(4.,0.,4.));
#17074=CARTESIAN_POINT('',(15.8288454112575,-0.000332254705457391,4.59484959654372));
#17075=CARTESIAN_POINT('',(15.7211545887425,-0.000419917270904514,4.59344262983929));
#17076=CARTESIAN_POINT('',(4.,-7.27562663373442E-17,4.5941));
#17077=CARTESIAN_POINT('Ctrl Pts',(15.8288454112575,-0.000332254705457391,
4.59484959654372));
#17078=CARTESIAN_POINT('Ctrl Pts',(15.814487640426,0.177680873019276,4.5936575613883));
#17079=CARTESIAN_POINT('Ctrl Pts',(15.8001298695944,0.356683508224643,4.50844978272675));
#17080=CARTESIAN_POINT('Ctrl Pts',(15.7857720987628,0.466927807092597,4.36891650689757));
#17081=CARTESIAN_POINT('Ctrl Pts',(15.7698668200752,0.589054446233417,4.21434406913608));
#17082=CARTESIAN_POINT('Ctrl Pts',(15.7539615413876,0.626802179063893,3.99310442736787));
#17083=CARTESIAN_POINT('Ctrl Pts',(15.7380562627,0.562838843643149,3.80678146521555));
#17084=CARTESIAN_POINT('Ctrl Pts',(15.7221509840123,0.498875508222402,3.62045850306322));
#17085=CARTESIAN_POINT('Ctrl Pts',(15.7062457053247,0.333201104550436,3.46905222052678));
#17086=CARTESIAN_POINT('Ctrl Pts',(15.6903404266371,0.141886309687413,3.42208197707538));
#17087=CARTESIAN_POINT('Ctrl Pts',(15.6744351479495,-0.0494284851756215,
3.37511173362399));
#17088=CARTESIAN_POINT('Ctrl Pts',(15.6585298692619,-0.266383671229707,
3.43257752925765));
#17089=CARTESIAN_POINT('Ctrl Pts',(15.6426245905743,-0.409362605655794,
3.5680935017987));
#17090=CARTESIAN_POINT('Ctrl Pts',(15.6267193118867,-0.552341540081869,
3.70360947433975));
#17091=CARTESIAN_POINT('Ctrl Pts',(15.6108140331991,-0.621344222879956,
3.9171756237882));
#17092=CARTESIAN_POINT('Ctrl Pts',(15.5949087545115,-0.584687541371933,
4.11073140955597));
#17093=CARTESIAN_POINT('Ctrl Pts',(15.5790034758238,-0.548030859863907,
4.30428719532377));
#17094=CARTESIAN_POINT('Ctrl Pts',(15.5630981971362,-0.405714814049763,
4.47783261741089));
#17095=CARTESIAN_POINT('Ctrl Pts',(15.5471929184486,-0.223084911271984,
4.55168296009627));
#17096=CARTESIAN_POINT('Ctrl Pts',(15.5410770827183,-0.152860773312716,
4.58007960584922));
#17097=CARTESIAN_POINT('Ctrl Pts',(15.5349612469879,-0.0766761255292402,
4.5937360717991));
#17098=CARTESIAN_POINT('Ctrl Pts',(15.5288454112575,-0.000350670266729247,
4.59332700645389));
#17099=CARTESIAN_POINT('Ctrl Pts',(15.4211545887425,0.000414092275955974,
4.59343115273787));
#17100=CARTESIAN_POINT('Ctrl Pts',(15.4313699441887,-0.12701715326484,4.59261555920332));
#17101=CARTESIAN_POINT('Ctrl Pts',(15.4415852996349,-0.254917899718674,
4.55240018390688));
#17102=CARTESIAN_POINT('Ctrl Pts',(15.4518006550811,-0.356261725310785,
4.47665348962993));
#17103=CARTESIAN_POINT('Ctrl Pts',(15.4677059337687,-0.514053766693778,
4.35871610717824));
#17104=CARTESIAN_POINT('Ctrl Pts',(15.4836112124564,-0.607465460011524,
4.15464228236211));
#17105=CARTESIAN_POINT('Ctrl Pts',(15.499516491144,-0.593606107615349,3.95813408188558));
#17106=CARTESIAN_POINT('Ctrl Pts',(15.5154217698316,-0.579746755219174,
3.76162588140906));
#17107=CARTESIAN_POINT('Ctrl Pts',(15.5313270485192,-0.458616357109098,
3.57268330527213));
#17108=CARTESIAN_POINT('Ctrl Pts',(15.5472323272068,-0.285832867492734,
3.47806079093568));
#17109=CARTESIAN_POINT('Ctrl Pts',(15.5631376058944,-0.113049377876356,
3.38343827659922));
#17110=CARTESIAN_POINT('Ctrl Pts',(15.579042884582,0.111387203246309,3.38313582406324));
#17111=CARTESIAN_POINT('Ctrl Pts',(15.5949481632696,0.284425092952457,3.47729230673655));
#17112=CARTESIAN_POINT('Ctrl Pts',(15.6108534419572,0.457462982658595,3.57144878940986));
#17113=CARTESIAN_POINT('Ctrl Pts',(15.6267587206449,0.579102180948212,3.76006420729246));
#17114=CARTESIAN_POINT('Ctrl Pts',(15.6426639993325,0.593491114096805,3.95653434015292));
#17115=CARTESIAN_POINT('Ctrl Pts',(15.6585692780201,0.607880047245398,4.15300447301339));
#17116=CARTESIAN_POINT('Ctrl Pts',(15.6744745567077,0.515018715252963,4.35732932085173));
#17117=CARTESIAN_POINT('Ctrl Pts',(15.6903798353953,0.357545113131455,4.47569155781202));
#17118=CARTESIAN_POINT('Ctrl Pts',(15.700638086511,0.255981111243369,4.55203033647815));
#17119=CARTESIAN_POINT('Ctrl Pts',(15.7108963376268,0.127540214881222,4.59261107697802));
#17120=CARTESIAN_POINT('Ctrl Pts',(15.7211545887425,-0.000419917270904514,
4.59344262983929));
#17121=CARTESIAN_POINT('Origin',(4.,0.,4.));
#17122=CARTESIAN_POINT('',(16.1288454112575,0.000520203518568921,4.59435747030618));
#17123=CARTESIAN_POINT('',(16.0211545887425,-0.00024144267326323,4.59496181546483));
#17124=CARTESIAN_POINT('',(4.,-7.27562663373442E-17,4.5941));
#17125=CARTESIAN_POINT('Ctrl Pts',(16.1288454112575,0.000520203518568921,
4.59435747030618));
#17126=CARTESIAN_POINT('Ctrl Pts',(16.1258245912393,0.0380542554257849,
4.59470210862833));
#17127=CARTESIAN_POINT('Ctrl Pts',(16.122803771221,0.0755288363057283,4.59145263304759));
#17128=CARTESIAN_POINT('Ctrl Pts',(16.1197829512027,0.112271568866026,4.58439375503351));
#17129=CARTESIAN_POINT('Ctrl Pts',(16.1038776725151,0.305730099191281,4.54722721702202));
#17130=CARTESIAN_POINT('Ctrl Pts',(16.0879723938275,0.478899942385972,4.40445440507416));
#17131=CARTESIAN_POINT('Ctrl Pts',(16.0720671151398,0.55226883266698,4.22163055421683));
#17132=CARTESIAN_POINT('Ctrl Pts',(16.0561618364522,0.625637722947984,4.03880670335952));
#17133=CARTESIAN_POINT('Ctrl Pts',(16.0402565577646,0.599205660315318,3.81593181359275));
#17134=CARTESIAN_POINT('Ctrl Pts',(16.024351279077,0.485109129681553,3.65534060523843));
#17135=CARTESIAN_POINT('Ctrl Pts',(16.0084460003894,0.371012599047788,3.4947493968841));
#17136=CARTESIAN_POINT('Ctrl Pts',(15.9925407217018,0.169251600412921,3.39644186994223));
#17137=CARTESIAN_POINT('Ctrl Pts',(15.9766354430142,-0.0275337514538456,
3.40555668173602));
#17138=CARTESIAN_POINT('Ctrl Pts',(15.9607301643265,-0.224319103320618,
3.41467149352982));
#17139=CARTESIAN_POINT('Ctrl Pts',(15.9448248856389,-0.416128808419276,
3.53120864405929));
#17140=CARTESIAN_POINT('Ctrl Pts',(15.9289196069513,-0.514891964967956,
3.70165920408156));
#17141=CARTESIAN_POINT('Ctrl Pts',(15.9130143282637,-0.613655121516638,
3.87210976410384));
#17142=CARTESIAN_POINT('Ctrl Pts',(15.8971090495761,-0.619371729515322,
4.09647373361892));
#17143=CARTESIAN_POINT('Ctrl Pts',(15.8812037708885,-0.52941696442075,4.27173266988224));
#17144=CARTESIAN_POINT('Ctrl Pts',(15.8652984922009,-0.439462199326184,
4.44699160614554));
#17145=CARTESIAN_POINT('Ctrl Pts',(15.8493932135132,-0.25383606113837,4.57314550915708));
#17146=CARTESIAN_POINT('Ctrl Pts',(15.8334879348256,-0.0577702193188812,
4.59226984378546));
#17147=CARTESIAN_POINT('Ctrl Pts',(15.8319404269696,-0.0386939468137543,
4.59413055045147));
#17148=CARTESIAN_POINT('Ctrl Pts',(15.8303929191136,-0.0195188482833839,
4.59497807636063));
#17149=CARTESIAN_POINT('Ctrl Pts',(15.8288454112575,-0.000332254705457391,
4.59484959654372));
#17150=CARTESIAN_POINT('Ctrl Pts',(15.7211545887425,-0.000419917270904514,
4.59344262983929));
#17151=CARTESIAN_POINT('Ctrl Pts',(15.7268016163144,-0.0708602278282204,
4.59390038836772));
#17152=CARTESIAN_POINT('Ctrl Pts',(15.7324486438863,-0.141154849878182,
4.58231274148771));
#17153=CARTESIAN_POINT('Ctrl Pts',(15.7380956714582,-0.206740066761224,
4.55801389847688));
#17154=CARTESIAN_POINT('Ctrl Pts',(15.7540009501458,-0.391465772281827,
4.48957437609924));
#17155=CARTESIAN_POINT('Ctrl Pts',(15.7699062288334,-0.538831311072463,
4.32029570526172));
#17156=CARTESIAN_POINT('Ctrl Pts',(15.785811507521,-0.58117266224226,4.12790349002296));
#17157=CARTESIAN_POINT('Ctrl Pts',(15.8017167862086,-0.62351401341206,3.93551127478418));
#17158=CARTESIAN_POINT('Ctrl Pts',(15.8176220648962,-0.560831176961022,
3.72000551514415));
#17159=CARTESIAN_POINT('Ctrl Pts',(15.8335273435838,-0.421905459495345,
3.58033733863277));
#17160=CARTESIAN_POINT('Ctrl Pts',(15.8494326222715,-0.282979742029676,
3.44066916212139));
#17161=CARTESIAN_POINT('Ctrl Pts',(15.8653379009591,-0.0678111435493865,
3.37683856873865));
#17162=CARTESIAN_POINT('Ctrl Pts',(15.8812431796467,0.124804018556085,3.41815386651619));
#17163=CARTESIAN_POINT('Ctrl Pts',(15.8971484583343,0.317419180661557,3.45946916429373));
#17164=CARTESIAN_POINT('Ctrl Pts',(15.9130537370219,0.487480906392202,3.60593035323155));
#17165=CARTESIAN_POINT('Ctrl Pts',(15.9289590157095,0.556904046010802,3.79028865163133));
#17166=CARTESIAN_POINT('Ctrl Pts',(15.9448642943971,0.6263271856294,3.9746469500311));
#17167=CARTESIAN_POINT('Ctrl Pts',(15.9607695730847,0.595111739135951,4.19690235789283));
#17168=CARTESIAN_POINT('Ctrl Pts',(15.9766748517723,0.477590518943614,4.35500459477727));
#17169=CARTESIAN_POINT('Ctrl Pts',(15.9915014307624,0.368039615220995,4.50238430120742));
#17170=CARTESIAN_POINT('Ctrl Pts',(16.0063280097524,0.18349252241573,4.59401752470064));
#17171=CARTESIAN_POINT('Ctrl Pts',(16.0211545887425,-0.00024144267326323,
4.59496181546483));
#17172=CARTESIAN_POINT('Origin',(4.,0.,4.));
#17173=CARTESIAN_POINT('',(16.4288454112575,7.48704377684928E-5,4.59312461313858));
#17174=CARTESIAN_POINT('',(16.3211545887425,0.000543344619121817,4.59417988242975));
#17175=CARTESIAN_POINT('',(4.,-7.27562663373442E-17,4.5941));
#17176=CARTESIAN_POINT('Ctrl Pts',(16.4288454112575,7.48704377684928E-5,
4.59312461313858));
#17177=CARTESIAN_POINT('Ctrl Pts',(16.4212562633649,0.0948679978941589,
4.5932308806522));
#17178=CARTESIAN_POINT('Ctrl Pts',(16.4136671154723,0.189615837117123,4.57184094704105));
#17179=CARTESIAN_POINT('Ctrl Pts',(16.4060779675797,0.273126642574496,4.52869916135151));
#17180=CARTESIAN_POINT('Ctrl Pts',(16.3901726888921,0.448147956300534,4.43828293357696));
#17181=CARTESIAN_POINT('Ctrl Pts',(16.3742674102045,0.573812330828296,4.25232504748949));
#17182=CARTESIAN_POINT('Ctrl Pts',(16.3583621315169,0.592420001795879,4.05620949715111));
#17183=CARTESIAN_POINT('Ctrl Pts',(16.3424568528292,0.611027672763462,3.86009394681272));
#17184=CARTESIAN_POINT('Ctrl Pts',(16.3265515741416,0.522578640170867,3.6538207322234));
#17185=CARTESIAN_POINT('Ctrl Pts',(16.310646295454,0.367684957814641,3.53210178682255));
#17186=CARTESIAN_POINT('Ctrl Pts',(16.2947410167664,0.212791275458425,3.4103828414217));
#17187=CARTESIAN_POINT('Ctrl Pts',(16.2788357380788,-0.00854705666138705,
3.3732181652093));
#17188=CARTESIAN_POINT('Ctrl Pts',(16.2629304593912,-0.19470084048803,3.43767220519428));
#17189=CARTESIAN_POINT('Ctrl Pts',(16.2470251807036,-0.380854624314662,
3.50212624517926));
#17190=CARTESIAN_POINT('Ctrl Pts',(16.231119902016,-0.531823859848111,3.66819900136163));
#17191=CARTESIAN_POINT('Ctrl Pts',(16.2152146233283,-0.578289861113055,
3.85963689006134));
#17192=CARTESIAN_POINT('Ctrl Pts',(16.1993093446407,-0.624755862378002,
4.05107477876107));
#17193=CARTESIAN_POINT('Ctrl Pts',(16.1834040659531,-0.566718629374431,
4.26787779997815));
#17194=CARTESIAN_POINT('Ctrl Pts',(16.1674987872655,-0.430826404144746,
4.41049917854914));
#17195=CARTESIAN_POINT('Ctrl Pts',(16.1546143285962,-0.320743594918802,
4.52603310245269));
#17196=CARTESIAN_POINT('Ctrl Pts',(16.1417298699269,-0.159570744489656,
4.592887512417));
#17197=CARTESIAN_POINT('Ctrl Pts',(16.1288454112575,0.000520203518568921,
4.59435747030618));
#17198=CARTESIAN_POINT('Ctrl Pts',(16.0211545887425,-0.00024144267326323,
4.59496181546483));
#17199=CARTESIAN_POINT('Ctrl Pts',(16.0222332884401,-0.0136089074611732,
4.59503051682625));
#17200=CARTESIAN_POINT('Ctrl Pts',(16.0233119881376,-0.0269720681925484,
4.59461918253551));
#17201=CARTESIAN_POINT('Ctrl Pts',(16.0243906878352,-0.0403017303441999,
4.59371435609144));
#17202=CARTESIAN_POINT('Ctrl Pts',(16.0402959665228,-0.236845765548457,
4.58037281461397));
#17203=CARTESIAN_POINT('Ctrl Pts',(16.0562012452104,-0.426106842065734,
4.45974066575184));
#17204=CARTESIAN_POINT('Ctrl Pts',(16.072106523898,-0.521184280535122,4.2872070887372));
#17205=CARTESIAN_POINT('Ctrl Pts',(16.0880118025856,-0.616261719004504,
4.11467351172257));
#17206=CARTESIAN_POINT('Ctrl Pts',(16.1039170812732,-0.61715551942601,3.89023850655542));
#17207=CARTESIAN_POINT('Ctrl Pts',(16.1198223599609,-0.523455286459661,
3.71695313254649));
#17208=CARTESIAN_POINT('Ctrl Pts',(16.1357276386485,-0.429755053493313,
3.54366775853756));
#17209=CARTESIAN_POINT('Ctrl Pts',(16.1516329173361,-0.241460787139106,
3.42153201568684));
#17210=CARTESIAN_POINT('Ctrl Pts',(16.1675381960237,-0.045029248433429,
3.40662546997421));
#17211=CARTESIAN_POINT('Ctrl Pts',(16.1834434747113,0.151402290272254,3.39171892426158));
#17212=CARTESIAN_POINT('Ctrl Pts',(16.1993487533989,0.355971101329402,3.48404157568705));
#17213=CARTESIAN_POINT('Ctrl Pts',(16.2152540320865,0.474747841293266,3.64120276856532));
#17214=CARTESIAN_POINT('Ctrl Pts',(16.2311593107741,0.593524581257127,3.79836396144359));
#17215=CARTESIAN_POINT('Ctrl Pts',(16.2470645894618,0.626509250127697,4.02036369577466));
#17216=CARTESIAN_POINT('Ctrl Pts',(16.2629698681494,0.558556683425868,4.20526908558792));
#17217=CARTESIAN_POINT('Ctrl Pts',(16.278875146837,0.490604116724039,4.39017447540119));
#17218=CARTESIAN_POINT('Ctrl Pts',(16.2947804255246,0.32171431444981,4.53798552069667));
#17219=CARTESIAN_POINT('Ctrl Pts',(16.3106857042122,0.129434328669215,4.58083364284428));
#17220=CARTESIAN_POINT('Ctrl Pts',(16.314175332389,0.0872479785030607,4.5902345478711));
#17221=CARTESIAN_POINT('Ctrl Pts',(16.3176649605657,0.0439357035691123,
4.5945828907904));
#17222=CARTESIAN_POINT('Ctrl Pts',(16.3211545887425,0.000543344619121817,
4.59417988242975));
#17223=CARTESIAN_POINT('Origin',(4.,0.,4.));
#17224=CARTESIAN_POINT('',(16.7288454112575,-0.000548108868865471,4.59408180714414));
#17225=CARTESIAN_POINT('',(16.6211545887425,-2.1752937549985E-5,4.5931168278739));
#17226=CARTESIAN_POINT('',(4.,-7.27562663373442E-17,4.5941));
#17227=CARTESIAN_POINT('Ctrl Pts',(16.7288454112575,-0.000548108868865471,
4.59408180714414));
#17228=CARTESIAN_POINT('Ctrl Pts',(16.7166879354906,0.15068989439403,4.59268722311157));
#17229=CARTESIAN_POINT('Ctrl Pts',(16.7045304597237,0.302891836883802,4.53390177381835));
#17230=CARTESIAN_POINT('Ctrl Pts',(16.6923729839567,0.411632901649024,4.42974331917764));
#17231=CARTESIAN_POINT('Ctrl Pts',(16.6764677052691,0.553895734249677,4.29347578465895));
#17232=CARTESIAN_POINT('Ctrl Pts',(16.6605624265815,0.621772048174623,4.07954898308531));
#17233=CARTESIAN_POINT('Ctrl Pts',(16.6446571478939,0.58409591167956,3.88618905124272));
#17234=CARTESIAN_POINT('Ctrl Pts',(16.6287518692063,0.546419775184499,3.69282911940014));
#17235=CARTESIAN_POINT('Ctrl Pts',(16.6128465905187,0.403191188269443,3.52003605728863));
#17236=CARTESIAN_POINT('Ctrl Pts',(16.596941311831,0.220174658543969,3.44714912875817));
#17237=CARTESIAN_POINT('Ctrl Pts',(16.5810360331434,0.0371581288184754,
3.37426220022769));
#17238=CARTESIAN_POINT('Ctrl Pts',(16.5651307544558,-0.185646343717467,
3.40128140527831));
#17239=CARTESIAN_POINT('Ctrl Pts',(16.5492254757682,-0.34593637135519,3.51580066803907));
#17240=CARTESIAN_POINT('Ctrl Pts',(16.5333201970806,-0.506226398992903,
3.63031993079982));
#17241=CARTESIAN_POINT('Ctrl Pts',(16.517414918393,-0.604001981732426,3.83233925127069));
#17242=CARTESIAN_POINT('Ctrl Pts',(16.5015096397054,-0.594368708523554,
4.02909990422408));
#17243=CARTESIAN_POINT('Ctrl Pts',(16.4856043610178,-0.584735435314682,
4.22586055717748));
#17244=CARTESIAN_POINT('Ctrl Pts',(16.4696990823301,-0.467693306157413,
4.4173625426134));
#17245=CARTESIAN_POINT('Ctrl Pts',(16.4537938036425,-0.296983115116624,
4.51567625060054));
#17246=CARTESIAN_POINT('Ctrl Pts',(16.4454776728475,-0.20772669247752,4.56707991793767));
#17247=CARTESIAN_POINT('Ctrl Pts',(16.4371615420525,-0.103798720846626,
4.59300816600183));
#17248=CARTESIAN_POINT('Ctrl Pts',(16.4288454112575,7.48704377684928E-5,
4.59312461313858));
#17249=CARTESIAN_POINT('Ctrl Pts',(16.3211545887425,0.000543344619121817,
4.59417988242975));
#17250=CARTESIAN_POINT('Ctrl Pts',(16.3335702392533,-0.153841115924154,
4.59274603025257));
#17251=CARTESIAN_POINT('Ctrl Pts',(16.3459858897642,-0.309239316255332,
4.53116741914846));
#17252=CARTESIAN_POINT('Ctrl Pts',(16.3584015402751,-0.418549561707542,
4.42300972860235));
#17253=CARTESIAN_POINT('Ctrl Pts',(16.3743068189627,-0.558583297016706,
4.28445249321304));
#17254=CARTESIAN_POINT('Ctrl Pts',(16.3902120976503,-0.622980598348072,
4.06945282343469));
#17255=CARTESIAN_POINT('Ctrl Pts',(16.4061173763379,-0.582172949355422,
3.87672947174358));
#17256=CARTESIAN_POINT('Ctrl Pts',(16.4220226550255,-0.541365300362771,
3.68400612005246));
#17257=CARTESIAN_POINT('Ctrl Pts',(16.4379279337131,-0.395352701046104,
3.5135590864486));
#17258=CARTESIAN_POINT('Ctrl Pts',(16.4538332124007,-0.211177959727979,
3.44365043774355));
#17259=CARTESIAN_POINT('Ctrl Pts',(16.4697384910883,-0.0270032184098532,
3.37374178903851));
#17260=CARTESIAN_POINT('Ctrl Pts',(16.485643769776,0.195333664909731,3.40437152523229));
#17261=CARTESIAN_POINT('Ctrl Pts',(16.5015490484636,0.353744999708243,3.52147576730199));
#17262=CARTESIAN_POINT('Ctrl Pts',(16.5174543271512,0.512156334506764,3.63858000937169));
#17263=CARTESIAN_POINT('Ctrl Pts',(16.5333596058388,0.606642120784206,3.84215875731731));
#17264=CARTESIAN_POINT('Ctrl Pts',(16.5492648845264,0.59381848284593,4.03873726278877));
#17265=CARTESIAN_POINT('Ctrl Pts',(16.565170163214,0.580994844907655,4.23531576826023));
#17266=CARTESIAN_POINT('Ctrl Pts',(16.5810754419016,0.460861782753675,4.42489403125753));
#17267=CARTESIAN_POINT('Ctrl Pts',(16.5969807205892,0.288579316114369,4.52042573380721));
#17268=CARTESIAN_POINT('Ctrl Pts',(16.6050386766403,0.201297315476928,4.56882414767653));
#17269=CARTESIAN_POINT('Ctrl Pts',(16.6130966326914,0.100630370301649,4.59308406930439));
#17270=CARTESIAN_POINT('Ctrl Pts',(16.6211545887425,-2.1752937549985E-5,
4.5931168278739));
#17271=CARTESIAN_POINT('Origin',(4.,0.,4.));
#17272=CARTESIAN_POINT('',(17.0288454112575,0.000186802344652959,4.59500977980842));
#17273=CARTESIAN_POINT('',(16.9211545887425,-0.000535257393875686,4.59425998651214));
#17274=CARTESIAN_POINT('',(4.,-7.27562663373442E-17,4.5941));
#17275=CARTESIAN_POINT('Ctrl Pts',(17.0288454112575,0.000186802344652959,
4.59500977980842));
#17276=CARTESIAN_POINT('Ctrl Pts',(17.0280248863039,0.0103527338555297,
4.59505157132578));
#17277=CARTESIAN_POINT('Ctrl Pts',(17.0272043613502,0.0205166685362397,
4.5948136789481));
#17278=CARTESIAN_POINT('Ctrl Pts',(17.0263838363966,0.0306658549750798,
4.59428997251885));
#17279=CARTESIAN_POINT('Ctrl Pts',(17.010478557709,0.227400443050786,4.58413830477164));
#17280=CARTESIAN_POINT('Ctrl Pts',(16.9945732790214,0.418593379366704,4.46659200952389));
#17281=CARTESIAN_POINT('Ctrl Pts',(16.9786680003338,0.516456956272638,4.29562337257973));
#17282=CARTESIAN_POINT('Ctrl Pts',(16.9627627216462,0.614320533178566,4.12465473563558));
#17283=CARTESIAN_POINT('Ctrl Pts',(16.9468574429585,0.618854750674521,3.90026375699502));
#17284=CARTESIAN_POINT('Ctrl Pts',(16.9309521642709,0.527977687913284,3.72548128085037));
#17285=CARTESIAN_POINT('Ctrl Pts',(16.9150468855833,0.437100625152047,3.55069880470573));
#17286=CARTESIAN_POINT('Ctrl Pts',(16.8991416068957,0.25081228213362,3.42552483105699));
#17287=CARTESIAN_POINT('Ctrl Pts',(16.8832363282081,0.054648384762208,3.40743395292956));
#17288=CARTESIAN_POINT('Ctrl Pts',(16.8673310495205,-0.141515512609204,
3.38934307480212));
#17289=CARTESIAN_POINT('Ctrl Pts',(16.8514257708328,-0.347554964333599,
3.47833529219599));
#17290=CARTESIAN_POINT('Ctrl Pts',(16.8355204921452,-0.468865370989487,
3.63354914383413));
#17291=CARTESIAN_POINT('Ctrl Pts',(16.8196152134576,-0.590175777645383,
3.78876299547228));
#17292=CARTESIAN_POINT('Ctrl Pts',(16.80370993477,-0.62675713923276,4.01019848135471));
#17293=CARTESIAN_POINT('Ctrl Pts',(16.7878046560824,-0.561812842140477,
4.19618179452704));
#17294=CARTESIAN_POINT('Ctrl Pts',(16.7718993773948,-0.496868545048197,
4.38216510769936));
#17295=CARTESIAN_POINT('Ctrl Pts',(16.7559940987072,-0.330398589276266,
4.53269624816158));
#17296=CARTESIAN_POINT('Ctrl Pts',(16.7400888200196,-0.138838935752124,
4.57865768466082));
#17297=CARTESIAN_POINT('Ctrl Pts',(16.7363410170989,-0.0937012275068688,
4.58948769960953));
#17298=CARTESIAN_POINT('Ctrl Pts',(16.7325932141782,-0.0471704703862807,
4.59451171761327));
#17299=CARTESIAN_POINT('Ctrl Pts',(16.7288454112575,-0.000548108868865471,
4.59408180714414));
#17300=CARTESIAN_POINT('Ctrl Pts',(16.6211545887425,-2.1752937549985E-5,
4.5931168278739));
#17301=CARTESIAN_POINT('Ctrl Pts',(16.629001911379,-0.0980428491191961,
4.59314873014073));
#17302=CARTESIAN_POINT('Ctrl Pts',(16.6368492340155,-0.196049888122182,
4.57020350190738));
#17303=CARTESIAN_POINT('Ctrl Pts',(16.6446965566521,-0.281666676968544,
4.52419924569128));
#17304=CARTESIAN_POINT('Ctrl Pts',(16.6606018353397,-0.455198332287519,
4.43095591292362));
#17305=CARTESIAN_POINT('Ctrl Pts',(16.6765071140273,-0.577829771800838,
4.24298410528626));
#17306=CARTESIAN_POINT('Ctrl Pts',(16.6924123927149,-0.593253826592341,
4.0465925244149));
#17307=CARTESIAN_POINT('Ctrl Pts',(16.7083176714025,-0.608677881383846,
3.85020094354353));
#17308=CARTESIAN_POINT('Ctrl Pts',(16.7242229500901,-0.516894551453523,
3.64538958943816));
#17309=CARTESIAN_POINT('Ctrl Pts',(16.7401282287778,-0.360046858872914,
3.52619917105016));
#17310=CARTESIAN_POINT('Ctrl Pts',(16.7560335074654,-0.203199166292313,
3.40700875266216));
#17311=CARTESIAN_POINT('Ctrl Pts',(16.771938786153,0.0187128889385656,3.37343926999153));
#17312=CARTESIAN_POINT('Ctrl Pts',(16.7878440648406,0.203796679382533,3.44090440927292));
#17313=CARTESIAN_POINT('Ctrl Pts',(16.8037493435282,0.388880469826499,3.50836954855431));
#17314=CARTESIAN_POINT('Ctrl Pts',(16.8196546222158,0.537135995483554,3.67686930978772));
#17315=CARTESIAN_POINT('Ctrl Pts',(16.8355599009034,0.58049059114602,3.86903573125179));
#17316=CARTESIAN_POINT('Ctrl Pts',(16.851465179591,0.623845186808487,4.06120215271587));
#17317=CARTESIAN_POINT('Ctrl Pts',(16.8673704582787,0.562298852476364,4.2770352344106));
#17318=CARTESIAN_POINT('Ctrl Pts',(16.8832757369663,0.424111061064287,4.41743355636644));
#17319=CARTESIAN_POINT('Ctrl Pts',(16.8959020208917,0.314411738992559,4.5288876912157));
#17320=CARTESIAN_POINT('Ctrl Pts',(16.9085283048171,0.156414067554279,4.59280392009262));
#17321=CARTESIAN_POINT('Ctrl Pts',(16.9211545887425,-0.000535257393875686,
4.59425998651214));
#17322=CARTESIAN_POINT('Origin',(4.,0.,4.));
#17323=CARTESIAN_POINT('',(17.3288454112575,0.000452601584348983,4.59351524744837));
#17324=CARTESIAN_POINT('',(17.2211545887425,0.000283723793354941,4.5949151055343));
#17325=CARTESIAN_POINT('',(4.,-7.27562663373442E-17,4.5941));
#17326=CARTESIAN_POINT('Ctrl Pts',(17.3288454112575,0.000452601584348983,
4.59351524744837));
#17327=CARTESIAN_POINT('Ctrl Pts',(17.3234565584296,0.0676518012035294,
4.59398979695312));
#17328=CARTESIAN_POINT('Ctrl Pts',(17.3180677056016,0.134706745978521,4.58346365752876));
#17329=CARTESIAN_POINT('Ctrl Pts',(17.3126788527736,0.197661386620268,4.56129398922237));
#17330=CARTESIAN_POINT('Ctrl Pts',(17.296773574086,0.383472937993069,4.49585988588324));
#17331=CARTESIAN_POINT('Ctrl Pts',(17.2808682953984,0.533564938357213,4.32899388620009));
#17332=CARTESIAN_POINT('Ctrl Pts',(17.2649630167108,0.579021491014364,4.13731379770915));
#17333=CARTESIAN_POINT('Ctrl Pts',(17.2490577380232,0.624478043671518,3.94563370921821));
#17334=CARTESIAN_POINT('Ctrl Pts',(17.2331524593355,0.565299148621668,3.72913953191949));
#17335=CARTESIAN_POINT('Ctrl Pts',(17.2172471806479,0.428657250819126,3.58723623291525));
#17336=CARTESIAN_POINT('Ctrl Pts',(17.2013419019603,0.292015353016592,3.44533293391101));
#17337=CARTESIAN_POINT('Ctrl Pts',(17.1854366232727,0.0779104524613767,
3.37802051320125));
#17338=CARTESIAN_POINT('Ctrl Pts',(17.1695313445851,-0.115349538542919,
3.41620598662221));
#17339=CARTESIAN_POINT('Ctrl Pts',(17.1536260658975,-0.308609529547215,
3.45439146004317));
#17340=CARTESIAN_POINT('Ctrl Pts',(17.1377207872099,-0.48102461100059,3.59807482759486));
#17341=CARTESIAN_POINT('Ctrl Pts',(17.1218155085223,-0.553429071780215,
3.78128276563952));
#17342=CARTESIAN_POINT('Ctrl Pts',(17.1059102298347,-0.625833532559839,
3.96449070368418));
#17343=CARTESIAN_POINT('Ctrl Pts',(17.090004951147,-0.598227372665711,4.18722321222181));
#17344=CARTESIAN_POINT('Ctrl Pts',(17.0740996724594,-0.483286172800906,
4.34721094636728));
#17345=CARTESIAN_POINT('Ctrl Pts',(17.0590149187255,-0.374274584390508,
4.4989451987145));
#17346=CARTESIAN_POINT('Ctrl Pts',(17.0439301649915,-0.186706445247169,
4.59424147319602));
#17347=CARTESIAN_POINT('Ctrl Pts',(17.0288454112575,0.000186802344652959,
4.59500977980842));
#17348=CARTESIAN_POINT('Ctrl Pts',(16.9211545887425,-0.000535257393875686,
4.59425998651214));
#17349=CARTESIAN_POINT('Ctrl Pts',(16.9244335835047,-0.0412943609811605,
4.59463812105998));
#17350=CARTESIAN_POINT('Ctrl Pts',(16.9277125782669,-0.0819827620002526,
4.59080381827239));
#17351=CARTESIAN_POINT('Ctrl Pts',(16.9309915730291,-0.121736182180322,
4.58249572362891));
#17352=CARTESIAN_POINT('Ctrl Pts',(16.9468968517167,-0.31456638552074,4.54219600671859));
#17353=CARTESIAN_POINT('Ctrl Pts',(16.9628021304043,-0.485397543709551,
4.39663301068103));
#17354=CARTESIAN_POINT('Ctrl Pts',(16.978707409092,-0.555791216176751,4.21264310503418));
#17355=CARTESIAN_POINT('Ctrl Pts',(16.9946126877796,-0.626184888643955,
4.02865319938731));
#17356=CARTESIAN_POINT('Ctrl Pts',(17.0105179664672,-0.596141075389537,
3.80623638413113));
#17357=CARTESIAN_POINT('Ctrl Pts',(17.0264232451548,-0.479454624411006,
3.64751705115182));
#17358=CARTESIAN_POINT('Ctrl Pts',(17.0423285238424,-0.362768173432475,
3.48879771817251));
#17359=CARTESIAN_POINT('Ctrl Pts',(17.05823380253,-0.159439084729831,3.39377586747005));
#17360=CARTESIAN_POINT('Ctrl Pts',(17.0741390812176,0.0371725263090214,
3.40608151284405));
#17361=CARTESIAN_POINT('Ctrl Pts',(17.0900443599052,0.233784137347885,3.41838715821804));
#17362=CARTESIAN_POINT('Ctrl Pts',(17.1059496385929,0.423678270722955,3.5380202996685));
#17363=CARTESIAN_POINT('Ctrl Pts',(17.1218549172805,0.519663574146654,3.71005045990219));
#17364=CARTESIAN_POINT('Ctrl Pts',(17.1377601959681,0.615648877570348,3.88208062013586));
#17365=CARTESIAN_POINT('Ctrl Pts',(17.1536654746557,0.617725351042682,4.10650779915277));
#17366=CARTESIAN_POINT('Ctrl Pts',(17.1695707533433,0.524939565793509,4.28028453107927));
#17367=CARTESIAN_POINT('Ctrl Pts',(17.1854760320309,0.432153780544336,4.45406126300578));
#17368=CARTESIAN_POINT('Ctrl Pts',(17.2013813107185,0.244505736573655,4.5771875478419));
#17369=CARTESIAN_POINT('Ctrl Pts',(17.2172865894061,0.0481554769387473,
4.59312900463441));
#17370=CARTESIAN_POINT('Ctrl Pts',(17.2185759225182,0.0322386925622284,
4.59442127046022));
#17371=CARTESIAN_POINT('Ctrl Pts',(17.2198652556304,0.0162647237884017,
4.5950091984451));
#17372=CARTESIAN_POINT('Ctrl Pts',(17.2211545887425,0.000283723793354941,
4.5949151055343));
#17373=CARTESIAN_POINT('Origin',(4.,0.,4.));
#17374=CARTESIAN_POINT('',(17.6288454112575,-0.000376811216598938,4.5933658344624));
#17375=CARTESIAN_POINT('',(17.5211545887425,0.000390292690419375,4.59338796628294));
#17376=CARTESIAN_POINT('',(4.,-7.27562663373442E-17,4.5941));
#17377=CARTESIAN_POINT('Ctrl Pts',(17.6288454112575,-0.000376811216598938,
4.5933658344624));
#17378=CARTESIAN_POINT('Ctrl Pts',(17.6188882305552,0.123868145157646,4.5926473455414));
#17379=CARTESIAN_POINT('Ctrl Pts',(17.608931049853,0.248515939035854,4.55458993700248));
#17380=CARTESIAN_POINT('Ctrl Pts',(17.5989738691507,0.348483110949462,4.48236965854082));
#17381=CARTESIAN_POINT('Ctrl Pts',(17.5830685904631,0.508167440925656,4.36700731952407));
#17382=CARTESIAN_POINT('Ctrl Pts',(17.5671633117754,0.604877102606476,4.16447556457896));
#17383=CARTESIAN_POINT('Ctrl Pts',(17.5512580330878,0.594207110796467,3.96776840716434));
#17384=CARTESIAN_POINT('Ctrl Pts',(17.5353527544002,0.583537118986457,3.77106124974973));
#17385=CARTESIAN_POINT('Ctrl Pts',(17.5194474757126,0.465487473685617,3.58017868986561));
#17386=CARTESIAN_POINT('Ctrl Pts',(17.503542197025,0.294261577747463,3.48276592343564));
#17387=CARTESIAN_POINT('Ctrl Pts',(17.4876369183374,0.123035681809298,3.38535315700567));
#17388=CARTESIAN_POINT('Ctrl Pts',(17.4717316396498,-0.101366464766187,
3.38141018402985));
#17389=CARTESIAN_POINT('Ctrl Pts',(17.4558263609621,-0.275908889943427,
3.47274745088526));
#17390=CARTESIAN_POINT('Ctrl Pts',(17.4399210822745,-0.450451315120656,
3.56408471774066));
#17391=CARTESIAN_POINT('Ctrl Pts',(17.4240158035869,-0.575134018899647,
3.75070222442727));
#17392=CARTESIAN_POINT('Ctrl Pts',(17.4081105248993,-0.592707978595278,
3.94691310701022));
#17393=CARTESIAN_POINT('Ctrl Pts',(17.3922052462117,-0.610281938290908,
4.14312398959316));
#17394=CARTESIAN_POINT('Ctrl Pts',(17.3762999675241,-0.520747153903178,
4.34892824807245));
#17395=CARTESIAN_POINT('Ctrl Pts',(17.3603946888365,-0.365214210518585,
4.46982927381454));
#17396=CARTESIAN_POINT('Ctrl Pts',(17.3498782629768,-0.262377240481122,
4.54976793433994));
#17397=CARTESIAN_POINT('Ctrl Pts',(17.3393618371172,-0.130687628661636,
4.59258915708319));
#17398=CARTESIAN_POINT('Ctrl Pts',(17.3288454112575,0.000452601584348983,
4.59351524744837));
#17399=CARTESIAN_POINT('Ctrl Pts',(17.2211545887425,0.000283723793354941,
4.5949151055343));
#17400=CARTESIAN_POINT('Ctrl Pts',(17.235770534318,-0.18087770297476,4.59384846352355));
#17401=CARTESIAN_POINT('Ctrl Pts',(17.2503864798935,-0.362942684182573,
4.50513801271133));
#17402=CARTESIAN_POINT('Ctrl Pts',(17.265002425469,-0.47285052735612,4.36129398677095));
#17403=CARTESIAN_POINT('Ctrl Pts',(17.2809077041566,-0.592453796716944,
4.20476088336606));
#17404=CARTESIAN_POINT('Ctrl Pts',(17.2968129828442,-0.626607860139456,
3.98293804780737));
#17405=CARTESIAN_POINT('Ctrl Pts',(17.3127182615318,-0.559630616639302,
3.79767714163318));
#17406=CARTESIAN_POINT('Ctrl Pts',(17.3286235402194,-0.492653373139145,
3.61241623545897));
#17407=CARTESIAN_POINT('Ctrl Pts',(17.3445288189071,-0.324544822716309,
3.46371725866926));
#17408=CARTESIAN_POINT('Ctrl Pts',(17.3604340975947,-0.132493299638714,
3.41985649047097));
#17409=CARTESIAN_POINT('Ctrl Pts',(17.3763393762823,0.0595582234388708,
3.37599572227269));
#17410=CARTESIAN_POINT('Ctrl Pts',(17.3922446549699,0.275552719171213,3.43697316266583));
#17411=CARTESIAN_POINT('Ctrl Pts',(17.4081499336575,0.416314653091553,3.5747905507646));
#17412=CARTESIAN_POINT('Ctrl Pts',(17.4240552123451,0.557076587011893,3.71260793886338));
#17413=CARTESIAN_POINT('Ctrl Pts',(17.4399604910327,0.622605959120231,3.92726527466781));
#17414=CARTESIAN_POINT('Ctrl Pts',(17.4558657697203,0.582814454063527,4.12020099097945));
#17415=CARTESIAN_POINT('Ctrl Pts',(17.4717710484079,0.543022949006823,4.31313670729109));
#17416=CARTESIAN_POINT('Ctrl Pts',(17.4876763270955,0.397910566785078,4.48435080410994));
#17417=CARTESIAN_POINT('Ctrl Pts',(17.5035816057832,0.214106774115907,4.55522901164789));
#17418=CARTESIAN_POINT('Ctrl Pts',(17.5094392667696,0.146414762764002,4.58133232736073));
#17419=CARTESIAN_POINT('Ctrl Pts',(17.515296927756,0.073474912906076,4.59382676872096));
#17420=CARTESIAN_POINT('Ctrl Pts',(17.5211545887425,0.000390292690419375,
4.59338796628294));
#17421=CARTESIAN_POINT('Origin',(4.,0.,4.));
#17422=CARTESIAN_POINT('',(17.9288454112575,-0.000301159635511528,4.59489313984584));
#17423=CARTESIAN_POINT('',(17.8211545887425,-0.000441626631060947,4.59348913571676));
#17424=CARTESIAN_POINT('',(4.,-7.27562663373442E-17,4.5941));
#17425=CARTESIAN_POINT('Ctrl Pts',(17.9288454112575,-0.000301159635511528,
4.59489313984584));
#17426=CARTESIAN_POINT('Ctrl Pts',(17.9143199026809,0.179756887528332,4.59377956832623));
#17427=CARTESIAN_POINT('Ctrl Pts',(17.8997943941043,0.360751589755073,4.50630604003092));
#17428=CARTESIAN_POINT('Ctrl Pts',(17.8852688855277,0.470789914960854,4.36397502945801));
#17429=CARTESIAN_POINT('Ctrl Pts',(17.8693636068401,0.591280720462369,4.20812407407766));
#17430=CARTESIAN_POINT('Ctrl Pts',(17.8534583281524,0.626694694978596,3.98649889312445));
#17431=CARTESIAN_POINT('Ctrl Pts',(17.8375530494648,0.560771239653389,3.80086039350393));
#17432=CARTESIAN_POINT('Ctrl Pts',(17.8216477707772,0.494847784328189,3.61522189388343));
#17433=CARTESIAN_POINT('Ctrl Pts',(17.8057424920896,0.327586899161578,3.46557007559562));
#17434=CARTESIAN_POINT('Ctrl Pts',(17.789837213402,0.135787706397568,3.42061872235194));
#17435=CARTESIAN_POINT('Ctrl Pts',(17.7739319347144,-0.0560114863664412,
3.37566736910827));
#17436=CARTESIAN_POINT('Ctrl Pts',(17.7580266560268,-0.272348986727849,
3.43541648090873));
#17437=CARTESIAN_POINT('Ctrl Pts',(17.7421213773392,-0.41389176700556,3.57243179339102));
#17438=CARTESIAN_POINT('Ctrl Pts',(17.7262160986515,-0.555434547283271,
3.7094471058733));
#17439=CARTESIAN_POINT('Ctrl Pts',(17.710310819964,-0.622182607477285,3.92372861903742));
#17440=CARTESIAN_POINT('Ctrl Pts',(17.6944055412763,-0.583488062224059,
4.11688732754162));
#17441=CARTESIAN_POINT('Ctrl Pts',(17.6785002625887,-0.544793516970831,
4.31004603604583));
#17442=CARTESIAN_POINT('Ctrl Pts',(17.6625949839011,-0.400656366270352,
4.48208193989012));
#17443=CARTESIAN_POINT('Ctrl Pts',(17.6466897052135,-0.217258291784321,
4.55400343026805));
#17444=CARTESIAN_POINT('Ctrl Pts',(17.6407416072282,-0.148672903323923,
4.58089991415997));
#17445=CARTESIAN_POINT('Ctrl Pts',(17.6347935092429,-0.0745967331795002,
4.59379503652584));
#17446=CARTESIAN_POINT('Ctrl Pts',(17.6288454112575,-0.000376811216598938,
4.5933658344624));
#17447=CARTESIAN_POINT('Ctrl Pts',(17.5211545887425,0.000390292690419375,
4.59338796628294));
#17448=CARTESIAN_POINT('Ctrl Pts',(17.5312022064437,-0.12497140465997,4.59263529057266));
#17449=CARTESIAN_POINT('Ctrl Pts',(17.5412498241448,-0.250759050797478,
4.55382993891589));
#17450=CARTESIAN_POINT('Ctrl Pts',(17.551297441846,-0.351218450958555,4.48038168762358));
#17451=CARTESIAN_POINT('Ctrl Pts',(17.5672027205336,-0.510244680247213,
4.36411383780432));
#17452=CARTESIAN_POINT('Ctrl Pts',(17.5831079992212,-0.605801935707933,
4.16103581990878));
#17453=CARTESIAN_POINT('Ctrl Pts',(17.5990132779088,-0.594014368327242,
3.96439246823218));
#17454=CARTESIAN_POINT('Ctrl Pts',(17.6149185565964,-0.58222680094655,3.76774911655557));
#17455=CARTESIAN_POINT('Ctrl Pts',(17.6308238352841,-0.463094410724447,
3.5775404310979));
#17456=CARTESIAN_POINT('Ctrl Pts',(17.6467291139717,-0.291317751175132,
3.48110219315546));
#17457=CARTESIAN_POINT('Ctrl Pts',(17.6626343926593,-0.119541091625818,
3.38466395521302));
#17458=CARTESIAN_POINT('Ctrl Pts',(17.6785396713469,0.104879837250709,3.38199616478582));
#17459=CARTESIAN_POINT('Ctrl Pts',(17.6944449500345,0.278900439380867,3.47432375837312));
#17460=CARTESIAN_POINT('Ctrl Pts',(17.7103502287221,0.452921041511034,3.56665135196042));
#17461=CARTESIAN_POINT('Ctrl Pts',(17.7262555074097,0.576541316894826,3.75397432956222));
#17462=CARTESIAN_POINT('Ctrl Pts',(17.7421607860974,0.593000065018554,3.95028190484542));
#17463=CARTESIAN_POINT('Ctrl Pts',(17.758066064785,0.60945881314228,4.1465894801286));
#17464=CARTESIAN_POINT('Ctrl Pts',(17.7739713434726,0.518756034005955,4.35188165309317));
#17465=CARTESIAN_POINT('Ctrl Pts',(17.7898766221602,0.362538606470845,4.47189694310939));
#17466=CARTESIAN_POINT('Ctrl Pts',(17.8003026110209,0.260137309937395,4.55056755941266));
#17467=CARTESIAN_POINT('Ctrl Pts',(17.8107285998817,0.129585238016204,4.59259583028147));
#17468=CARTESIAN_POINT('Ctrl Pts',(17.8211545887425,-0.000441626631060947,
4.59348913571676));
#17469=CARTESIAN_POINT('Origin',(4.,0.,4.));
#17470=CARTESIAN_POINT('',(18.2288454112575,0.000530626821107938,4.59429426521737));
#17471=CARTESIAN_POINT('',(18.1211545887425,-0.000206261771334874,4.59499421029555));
#17472=CARTESIAN_POINT('',(4.,-7.27562663373442E-17,4.5941));
#17473=CARTESIAN_POINT('Ctrl Pts',(18.2288454112575,0.000530626821107938,
4.59429426521737));
#17474=CARTESIAN_POINT('Ctrl Pts',(18.2256568534942,0.0401596894680921,
4.59466101186164));
#17475=CARTESIAN_POINT('Ctrl Pts',(18.2224682957309,0.0797220295111884,
4.5910372210354));
#17476=CARTESIAN_POINT('Ctrl Pts',(18.2192797379675,0.118424305077702,4.58317806034235));
#17477=CARTESIAN_POINT('Ctrl Pts',(18.2033744592799,0.311480390123117,4.54397471188459));
#17478=CARTESIAN_POINT('Ctrl Pts',(18.1874691805923,0.483135922039688,4.39938477867344));
#17479=CARTESIAN_POINT('Ctrl Pts',(18.1715639019047,0.554573942717995,4.21579784094385));
#17480=CARTESIAN_POINT('Ctrl Pts',(18.1556586232171,0.626011963396302,4.03221090321426));
#17481=CARTESIAN_POINT('Ctrl Pts',(18.1397533445295,0.597232472836345,3.80962696096622));
#17482=CARTESIAN_POINT('Ctrl Pts',(18.1238480658419,0.481449795543417,3.65024714373002));
#17483=CARTESIAN_POINT('Ctrl Pts',(18.1079427871543,0.365667118250483,3.49086732649381));
#17484=CARTESIAN_POINT('Ctrl Pts',(18.0920375084667,0.16288125422457,3.39469163426944));
#17485=CARTESIAN_POINT('Ctrl Pts',(18.076132229779,-0.0337971069360236,
3.40587987606835));
#17486=CARTESIAN_POINT('Ctrl Pts',(18.0602269510914,-0.230475468096606,
3.41706811786726));
#17487=CARTESIAN_POINT('Ctrl Pts',(18.0443216724038,-0.421046326391869,
3.53562029368944));
#17488=CARTESIAN_POINT('Ctrl Pts',(18.0284163937162,-0.518007606080761,
3.70710225992629));
#17489=CARTESIAN_POINT('Ctrl Pts',(18.0125111150286,-0.614968885769652,
3.87858422616314));
#17490=CARTESIAN_POINT('Ctrl Pts',(17.996605836341,-0.618320586852172,4.10299598281466));
#17491=CARTESIAN_POINT('Ctrl Pts',(17.9807005576534,-0.526523749990007,
4.27729714530494));
#17492=CARTESIAN_POINT('Ctrl Pts',(17.9647952789658,-0.434726913127837,
4.45159830779523));
#17493=CARTESIAN_POINT('Ctrl Pts',(17.9488900002781,-0.247781538320971,
4.57578887612429));
#17494=CARTESIAN_POINT('Ctrl Pts',(17.9329847215905,-0.0515250326741526,
4.59284579538505));
#17495=CARTESIAN_POINT('Ctrl Pts',(17.9316049514795,-0.0344999389365885,
4.59432546938787));
#17496=CARTESIAN_POINT('Ctrl Pts',(17.9302251813685,-0.0174047750035579,
4.59499891739512));
#17497=CARTESIAN_POINT('Ctrl Pts',(17.9288454112575,-0.000301159635511528,
4.59489313984584));
#17498=CARTESIAN_POINT('Ctrl Pts',(17.8211545887425,-0.000441626631060947,
4.59348913571676));
#17499=CARTESIAN_POINT('Ctrl Pts',(17.8266338785693,-0.0687761401428734,
4.59395860479535));
#17500=CARTESIAN_POINT('Ctrl Pts',(17.8321131683962,-0.136965594625977,
4.58306684864343));
#17501=CARTESIAN_POINT('Ctrl Pts',(17.837592458223,-0.200847632772524,4.56016175744822));
#17502=CARTESIAN_POINT('Ctrl Pts',(17.8534977369106,-0.386284368546891,
4.49367287470298));
#17503=CARTESIAN_POINT('Ctrl Pts',(17.8694030155983,-0.535425764161732,
4.32595670214462));
#17504=CARTESIAN_POINT('Ctrl Pts',(17.8853082942859,-0.579792400402821,
4.13402141072584));
#17505=CARTESIAN_POINT('Ctrl Pts',(17.9012135729735,-0.624159036643913,
3.94208611930704));
#17506=CARTESIAN_POINT('Ctrl Pts',(17.9171188516611,-0.563750913511241,
3.72593170902781));
#17507=CARTESIAN_POINT('Ctrl Pts',(17.9330241303487,-0.426304885490399,
3.58480714034942));
#17508=CARTESIAN_POINT('Ctrl Pts',(17.9489294090363,-0.288858857469565,
3.44368257167104));
#17509=CARTESIAN_POINT('Ctrl Pts',(17.9648346877239,-0.0743749245605683,
3.37758784459349));
#17510=CARTESIAN_POINT('Ctrl Pts',(17.9807399664116,0.118664965311668,3.41687086155347));
#17511=CARTESIAN_POINT('Ctrl Pts',(17.9966452450992,0.311704855183904,3.45615387851346));
#17512=CARTESIAN_POINT('Ctrl Pts',(18.0125505237868,0.483300702019379,3.60081463951098));
#17513=CARTESIAN_POINT('Ctrl Pts',(18.0284558024744,0.554662952572844,3.78443104318807));
#17514=CARTESIAN_POINT('Ctrl Pts',(18.044361081162,0.62602520312631,3.96804744686516));
#17515=CARTESIAN_POINT('Ctrl Pts',(18.0602663598496,0.597153857397765,4.19061949322182));
#17516=CARTESIAN_POINT('Ctrl Pts',(18.0761716385372,0.481305415899848,4.34995151481781));
#17517=CARTESIAN_POINT('Ctrl Pts',(18.0911659552723,0.372092100044007,4.50015792394613));
#17518=CARTESIAN_POINT('Ctrl Pts',(18.1061602720074,0.185579460002099,4.59416090236354));
#17519=CARTESIAN_POINT('Ctrl Pts',(18.1211545887425,-0.000206261771334874,
4.59499421029555));
#17520=CARTESIAN_POINT('Origin',(4.,0.,4.));
#17521=CARTESIAN_POINT('',(18.5288454112575,4.04073003155148E-5,4.59311858068669));
#17522=CARTESIAN_POINT('',(18.4211545887425,0.000547083855738422,4.59411609730493));
#17523=CARTESIAN_POINT('',(4.,-7.27562663373442E-17,4.5941));
#17524=CARTESIAN_POINT('Ctrl Pts',(18.5288454112575,4.04073003155148E-5,
4.59311858068669));
#17525=CARTESIAN_POINT('Ctrl Pts',(18.5210885256199,0.0969311390001333,
4.59317716754242));
#17526=CARTESIAN_POINT('Ctrl Pts',(18.5133316399822,0.193796352446061,4.57078374547556));
#17527=CARTESIAN_POINT('Ctrl Pts',(18.5055747543446,0.27868347559656,4.52579129559858));
#17528=CARTESIAN_POINT('Ctrl Pts',(18.489669475657,0.452742165355285,4.43353552600749));
#17529=CARTESIAN_POINT('Ctrl Pts',(18.4737641969693,0.576439736070726,4.24626358090446));
#17530=CARTESIAN_POINT('Ctrl Pts',(18.4578589182817,0.592979496483005,4.04996281465819));
#17531=CARTESIAN_POINT('Ctrl Pts',(18.4419536395941,0.609519256895283,3.85366204841193));
#17532=CARTESIAN_POINT('Ctrl Pts',(18.4260483609065,0.518901207004412,3.64833246102244));
#17533=CARTESIAN_POINT('Ctrl Pts',(18.4101430822189,0.362733321586741,3.52825271224048));
#17534=CARTESIAN_POINT('Ctrl Pts',(18.3942378035313,0.206565436169079,3.40817296345854));
#17535=CARTESIAN_POINT('Ctrl Pts',(18.3783325248437,-0.015152284775374,
3.37334305328413));
#17536=CARTESIAN_POINT('Ctrl Pts',(18.3624272461561,-0.200616443892158,
3.43975540293737));
#17537=CARTESIAN_POINT('Ctrl Pts',(18.3465219674685,-0.386080603008964,
3.50616775259061));
#17538=CARTESIAN_POINT('Ctrl Pts',(18.3306166887808,-0.535291200298091,
3.67382236207151));
#17539=CARTESIAN_POINT('Ctrl Pts',(18.3147114100932,-0.579737042064157,
3.86573932758804));
#17540=CARTESIAN_POINT('Ctrl Pts',(18.2988061314056,-0.624182883830224,
4.05765629310458));
#17541=CARTESIAN_POINT('Ctrl Pts',(18.282900852718,-0.563863970073232,4.27383561465674));
#17542=CARTESIAN_POINT('Ctrl Pts',(18.2669955740304,-0.426476194107598,
4.41501689358062));
#17543=CARTESIAN_POINT('Ctrl Pts',(18.2542788531061,-0.316630774880643,
4.52789532589669));
#17544=CARTESIAN_POINT('Ctrl Pts',(18.2415621321818,-0.157519428275204,
4.5928315930404));
#17545=CARTESIAN_POINT('Ctrl Pts',(18.2288454112575,0.000530626821107938,
4.59429426521737));
#17546=CARTESIAN_POINT('Ctrl Pts',(18.1211545887425,-0.000206261771334874,
4.59499421029555));
#17547=CARTESIAN_POINT('Ctrl Pts',(18.122065550695,-0.0114934532352288,
4.59504483693191));
#17548=CARTESIAN_POINT('Ctrl Pts',(18.1229765126475,-0.0227779616248223,
4.59475157188293));
#17549=CARTESIAN_POINT('Ctrl Pts',(18.1238874746001,-0.0340422900297544,
4.59410612569417));
#17550=CARTESIAN_POINT('Ctrl Pts',(18.1397927532877,-0.230716017194119,
4.58283671813918));
#17551=CARTESIAN_POINT('Ctrl Pts',(18.1556980319753,-0.421237934255556,
4.46420590619388));
#17552=CARTESIAN_POINT('Ctrl Pts',(18.1716033106629,-0.518128437217054,
4.29268393984778));
#17553=CARTESIAN_POINT('Ctrl Pts',(18.1875085893505,-0.615018940178556,
4.12116197350168));
#17554=CARTESIAN_POINT('Ctrl Pts',(18.2034138680381,-0.618278029040109,
3.89674885275477));
#17555=CARTESIAN_POINT('Ctrl Pts',(18.2193191467258,-0.526409268077163,
3.72248558851787));
#17556=CARTESIAN_POINT('Ctrl Pts',(18.2352244254134,-0.434540507114227,
3.54822232428098));
#17557=CARTESIAN_POINT('Ctrl Pts',(18.251129704101,-0.24754389632682,3.42410891655409));
#17558=CARTESIAN_POINT('Ctrl Pts',(18.2670349827886,-0.0512803682143169,
3.40713299136011));
#17559=CARTESIAN_POINT('Ctrl Pts',(18.2829402614762,0.144983159898198,3.39015706616613));
#17560=CARTESIAN_POINT('Ctrl Pts',(18.2988455401638,0.35051360533581,3.48031862350507));
#17561=CARTESIAN_POINT('Ctrl Pts',(18.3147508188514,0.470940082829639,3.63621929066782));
#17562=CARTESIAN_POINT('Ctrl Pts',(18.330656097539,0.591366560323475,3.79211995783059));
#17563=CARTESIAN_POINT('Ctrl Pts',(18.3465613762266,0.62668906987352,4.01375973481717));
#17564=CARTESIAN_POINT('Ctrl Pts',(18.3624666549143,0.560689009466533,4.199371012841));
#17565=CARTESIAN_POINT('Ctrl Pts',(18.3783719336019,0.49468894905955,4.38498229086483));
#17566=CARTESIAN_POINT('Ctrl Pts',(18.3942772122895,0.327366318695548,4.53456506992591));
#17567=CARTESIAN_POINT('Ctrl Pts',(18.4101824909771,0.135548591400956,4.57943726620491));
#17568=CARTESIAN_POINT('Ctrl Pts',(18.4138398568989,0.0914407431336166,
4.58975547846199));
#17569=CARTESIAN_POINT('Ctrl Pts',(18.4174972228207,0.0460377050408626,
4.59453706917327));
#17570=CARTESIAN_POINT('Ctrl Pts',(18.4211545887425,0.000547083855738422,
4.59411609730493));
#17571=CARTESIAN_POINT('Origin',(4.,0.,4.));
#17572=CARTESIAN_POINT('',(18.8288454112575,-0.000545657836941327,4.59414547262434));
#17573=CARTESIAN_POINT('',(18.7211545887425,-5.63168744233308E-5,4.59312091231189));
#17574=CARTESIAN_POINT('',(4.,-7.27562663373442E-17,4.5941));
#17575=CARTESIAN_POINT('Ctrl Pts',(18.8288454112575,-0.000545657836941327,
4.59414547262434));
#17576=CARTESIAN_POINT('Ctrl Pts',(18.8165201977456,0.15273698101805,4.59272393327212));
#17577=CARTESIAN_POINT('Ctrl Pts',(18.8041949842336,0.307016766534516,4.53213273669464));
#17578=CARTESIAN_POINT('Ctrl Pts',(18.7918697707216,0.416139138999065,4.42538122089617));
#17579=CARTESIAN_POINT('Ctrl Pts',(18.775964492034,0.556957936451544,4.28762193522949));
#17580=CARTESIAN_POINT('Ctrl Pts',(18.7600592133464,0.622575889387102,4.0729916608594));
#17581=CARTESIAN_POINT('Ctrl Pts',(18.7441539346588,0.582864009884755,3.88003953951897));
#17582=CARTESIAN_POINT('Ctrl Pts',(18.7282486559712,0.543152130382401,3.6870874181785));
#17583=CARTESIAN_POINT('Ctrl Pts',(18.7123433772835,0.3981104184421,3.51581344986768));
#17584=CARTESIAN_POINT('Ctrl Pts',(18.6964380985959,0.214335891977863,3.44485939483061));
#17585=CARTESIAN_POINT('Ctrl Pts',(18.6805328199083,0.0305613655136472,
3.37390533979354));
#17586=CARTESIAN_POINT('Ctrl Pts',(18.6646275412207,-0.191945975474496,
3.40327119803019));
#17587=CARTESIAN_POINT('Ctrl Pts',(18.6487222625331,-0.351020173514001,
3.51947340980541));
#17588=CARTESIAN_POINT('Ctrl Pts',(18.6328169838455,-0.510094371553506,
3.63567562158063));
#17589=CARTESIAN_POINT('Ctrl Pts',(18.6169117051579,-0.605735426644373,
3.83871418689441));
#17590=CARTESIAN_POINT('Ctrl Pts',(18.6010064264702,-0.594029012528289,
4.03536238640794));
#17591=CARTESIAN_POINT('Ctrl Pts',(18.5851011477826,-0.582322598412206,
4.23201058592146));
#17592=CARTESIAN_POINT('Ctrl Pts',(18.569195869095,-0.463268715089173,4.42226841963472));
#17593=CARTESIAN_POINT('Ctrl Pts',(18.5532905904074,-0.29153186902666,4.51877753945177));
#17594=CARTESIAN_POINT('Ctrl Pts',(18.5451421973574,-0.203549800283198,
4.56821988225003));
#17595=CARTESIAN_POINT('Ctrl Pts',(18.5369938043075,-0.101740616897797,
4.59305703682098));
#17596=CARTESIAN_POINT('Ctrl Pts',(18.5288454112575,4.04073003155148E-5,
4.59311858068669));
#17597=CARTESIAN_POINT('Ctrl Pts',(18.4211545887425,0.000547083855738422,
4.59411609730493));
#17598=CARTESIAN_POINT('Ctrl Pts',(18.4334025015083,-0.151793472668411,
4.59270633223614));
#17599=CARTESIAN_POINT('Ctrl Pts',(18.4456504142741,-0.305116246576315,
4.53295143150856));
#17600=CARTESIAN_POINT('Ctrl Pts',(18.4578983270399,-0.414068183831284,
4.42739736222451));
#17601=CARTESIAN_POINT('Ctrl Pts',(18.4738036057275,-0.555554407543751,
4.29032364846819));
#17602=CARTESIAN_POINT('Ctrl Pts',(18.4897088844152,-0.622214030743504,
4.07601460745865));
#17603=CARTESIAN_POINT('Ctrl Pts',(18.5056141631028,-0.583439774593308,
3.88287188415962));
#17604=CARTESIAN_POINT('Ctrl Pts',(18.5215194417904,-0.54466551844311,3.68972916086059));
#17605=CARTESIAN_POINT('Ctrl Pts',(18.537424720478,-0.400457382942952,3.51775275527208));
#17606=CARTESIAN_POINT('Ctrl Pts',(18.5533299991656,-0.217029642971419,
3.44590695711865));
#17607=CARTESIAN_POINT('Ctrl Pts',(18.5692352778532,-0.0336019029998957,
3.37406115896522));
#17608=CARTESIAN_POINT('Ctrl Pts',(18.5851405565408,0.189045441442997,3.40234596824686));
#17609=CARTESIAN_POINT('Ctrl Pts',(18.6010458352284,0.348682149221421,3.51777419717301));
#17610=CARTESIAN_POINT('Ctrl Pts',(18.6169511139161,0.508318856999844,3.63320242609916));
#17611=CARTESIAN_POINT('Ctrl Pts',(18.6328563926037,0.604944928113798,3.83577407466982));
#17612=CARTESIAN_POINT('Ctrl Pts',(18.6487616712913,0.594193758619731,4.03247681196108));
#17613=CARTESIAN_POINT('Ctrl Pts',(18.6646669499789,0.583442589125664,4.22917954925235));
#17614=CARTESIAN_POINT('Ctrl Pts',(18.6805722286665,0.465314179023576,4.42001337526422));
#17615=CARTESIAN_POINT('Ctrl Pts',(18.6964775073541,0.294048096631404,4.51735547060535));
#17616=CARTESIAN_POINT('Ctrl Pts',(18.7047032011502,0.205474838715737,4.56769764225005));
#17617=CARTESIAN_POINT('Ctrl Pts',(18.7129288949463,0.102689258835563,4.59303430424318));
#17618=CARTESIAN_POINT('Ctrl Pts',(18.7211545887425,-5.63168744233308E-5,
4.59312091231189));
#17619=CARTESIAN_POINT('Origin',(4.,0.,4.));
#17620=CARTESIAN_POINT('',(19.1288454112575,0.000222628893785728,4.59497983522242));
#17621=CARTESIAN_POINT('',(19.0211545887425,-0.000526118841417405,4.59432346427954));
#17622=CARTESIAN_POINT('',(4.,-7.27562663373442E-17,4.5941));
#17623=CARTESIAN_POINT('Ctrl Pts',(19.1288454112575,0.000222628893785728,
4.59497983522242));
#17624=CARTESIAN_POINT('Ctrl Pts',(19.1278571485589,0.012468395078646,4.59503853204781));
#17625=CARTESIAN_POINT('Ctrl Pts',(19.1268688858602,0.0247107891953784,
4.59469333777414));
#17626=CARTESIAN_POINT('Ctrl Pts',(19.1258806231615,0.0369274203756033,
4.59393377720877));
#17627=CARTESIAN_POINT('Ctrl Pts',(19.1099753444739,0.233544093050454,4.58170927203582));
#17628=CARTESIAN_POINT('Ctrl Pts',(19.0940700657862,0.423487581379576,4.46215450773496));
#17629=CARTESIAN_POINT('Ctrl Pts',(19.0781647870986,0.519543871337238,4.29016397409385));
#17630=CARTESIAN_POINT('Ctrl Pts',(19.062259508411,0.615600161294901,4.11817344045274));
#17631=CARTESIAN_POINT('Ctrl Pts',(19.0463542297234,0.617769252881104,3.89374713747137));
#17632=CARTESIAN_POINT('Ctrl Pts',(19.0304489510358,0.525055191022736,3.71993212880311));
#17633=CARTESIAN_POINT('Ctrl Pts',(19.0145436723482,0.432341129164367,3.54611712013485));
#17634=CARTESIAN_POINT('Ctrl Pts',(18.9986383936606,0.244743913861428,3.42291340577968));
#17635=CARTESIAN_POINT('Ctrl Pts',(18.982733114973,0.0484002497885746,3.40689091904056));
#17636=CARTESIAN_POINT('Ctrl Pts',(18.9668278362853,-0.147943414284278,
3.39086843230144));
#17637=CARTESIAN_POINT('Ctrl Pts',(18.9509225575977,-0.353033527127044,
3.48202717317836));
#17638=CARTESIAN_POINT('Ctrl Pts',(18.9350172789101,-0.472701385564812,
3.63851090447403));
#17639=CARTESIAN_POINT('Ctrl Pts',(18.9191120002225,-0.592369244002587,
3.79499463576972));
#17640=CARTESIAN_POINT('Ctrl Pts',(18.9032067215349,-0.626614848035354,
4.01680335748416));
#17641=CARTESIAN_POINT('Ctrl Pts',(18.8873014428473,-0.559714065105754,
4.20209188855652));
#17642=CARTESIAN_POINT('Ctrl Pts',(18.8713961641597,-0.492813282176159,
4.38738041962887));
#17643=CARTESIAN_POINT('Ctrl Pts',(18.8554908854721,-0.324766112284209,
4.53614876005914));
#17644=CARTESIAN_POINT('Ctrl Pts',(18.8395856067844,-0.132732706353525,
4.58008878179264));
#17645=CARTESIAN_POINT('Ctrl Pts',(18.8360055416088,-0.0895085590353085,
4.5899790920924));
#17646=CARTESIAN_POINT('Ctrl Pts',(18.8324254764332,-0.0450691735440342,
4.59455838259347));
#17647=CARTESIAN_POINT('Ctrl Pts',(18.8288454112575,-0.000545657836941327,
4.59414547262434));
#17648=CARTESIAN_POINT('Ctrl Pts',(18.7211545887425,-5.63168744233308E-5,
4.59312091231189));
#17649=CARTESIAN_POINT('Ctrl Pts',(18.728834173634,-0.0959805501911411,
4.59320177041728));
#17650=CARTESIAN_POINT('Ctrl Pts',(18.7365137585255,-0.191869914813978,
4.57127401300463));
#17651=CARTESIAN_POINT('Ctrl Pts',(18.744193343417,-0.276126457005151,4.5271386400555));
#17652=CARTESIAN_POINT('Ctrl Pts',(18.7600986221046,-0.450631173567243,
4.43572934949413));
#17653=CARTESIAN_POINT('Ctrl Pts',(18.7760039007922,-0.575236852009173,
4.249060403701));
#17654=CARTESIAN_POINT('Ctrl Pts',(18.7919091794798,-0.592729836422094,
4.05284228527226));
#17655=CARTESIAN_POINT('Ctrl Pts',(18.8078144581674,-0.610222820835014,
3.85662416684351));
#17656=CARTESIAN_POINT('Ctrl Pts',(18.823719736855,-0.520603111218926,3.65085687577915));
#17657=CARTESIAN_POINT('Ctrl Pts',(18.8396250155426,-0.365020286731977,
3.53002004684018));
#17658=CARTESIAN_POINT('Ctrl Pts',(18.8555302942302,-0.209437462245028,
3.40918321790122));
#17659=CARTESIAN_POINT('Ctrl Pts',(18.8714355729179,0.0121084771127808,
3.37327685108765));
#17660=CARTESIAN_POINT('Ctrl Pts',(18.8873408516055,0.197893008823487,3.43878763096633));
#17661=CARTESIAN_POINT('Ctrl Pts',(18.9032461302931,0.383677540534204,3.50429841084501));
#17662=CARTESIAN_POINT('Ctrl Pts',(18.9191514089807,0.533700664597814,3.67122633741595));
#17663=CARTESIAN_POINT('Ctrl Pts',(18.9350566876683,0.579078109400399,3.86292516893752));
#17664=CARTESIAN_POINT('Ctrl Pts',(18.9509619663559,0.624455554202981,4.05462400045908));
#17665=CARTESIAN_POINT('Ctrl Pts',(18.9668672450435,0.56518731974455,4.27109373693126));
#17666=CARTESIAN_POINT('Ctrl Pts',(18.9827725237311,0.428486871854059,4.41294063344238));
#17667=CARTESIAN_POINT('Ctrl Pts',(18.9955665454016,0.318526617336051,4.52704063153052));
#17668=CARTESIAN_POINT('Ctrl Pts',(19.008360567072,0.158464569423419,4.5928566151945));
#17669=CARTESIAN_POINT('Ctrl Pts',(19.0211545887425,-0.000526118841417405,
4.59432346427954));
#17670=CARTESIAN_POINT('Origin',(4.,0.,4.));
#17671=CARTESIAN_POINT('',(19.4288454112575,0.000431836873498515,4.59346738712276));
#17672=CARTESIAN_POINT('',(19.3211545887425,0.000315695961457875,4.59487351203822));
#17673=CARTESIAN_POINT('',(4.,-7.27562663373442E-17,4.5941));
#17674=CARTESIAN_POINT('Ctrl Pts',(19.4288454112575,0.000431836873498515,
4.59346738712276));
#17675=CARTESIAN_POINT('Ctrl Pts',(19.4232888206845,0.0697367837969298,
4.59393182999066));
#17676=CARTESIAN_POINT('Ctrl Pts',(19.4177322301115,0.13889623855249,4.58272225272434));
#17677=CARTESIAN_POINT('Ctrl Pts',(19.4121756395385,0.203565929825556,4.55917964700716));
#17678=CARTESIAN_POINT('Ctrl Pts',(19.3962703608509,0.38867754617092,4.49179089484985));
#17679=CARTESIAN_POINT('Ctrl Pts',(19.3803650821633,0.537002597765565,4.32335233206236));
#17680=CARTESIAN_POINT('Ctrl Pts',(19.3644598034757,0.580436494614329,4.13120381907284));
#17681=CARTESIAN_POINT('Ctrl Pts',(19.3485545247881,0.623870391463095,3.93905530608331));
#17682=CARTESIAN_POINT('Ctrl Pts',(19.3326492461004,0.562413133565966,3.72319684289176));
#17683=CARTESIAN_POINT('Ctrl Pts',(19.3167439674128,0.424283294458304,3.58274150440131));
#17684=CARTESIAN_POINT('Ctrl Pts',(19.3008386887252,0.286153455350651,3.44228616591086));
#17685=CARTESIAN_POINT('Ctrl Pts',(19.2849334100376,0.071351035032473,3.37723395212151));
#17686=CARTESIAN_POINT('Ctrl Pts',(19.26902813135,-0.12149578302492,3.4174540870367));
#17687=CARTESIAN_POINT('Ctrl Pts',(19.2531228526624,-0.314342601082313,
3.45767422195189));
#17688=CARTESIAN_POINT('Ctrl Pts',(19.2372175739748,-0.485233816878921,
3.60316670557164));
#17689=CARTESIAN_POINT('Ctrl Pts',(19.2213122952871,-0.555703413721375,
3.78712754492824));
#17690=CARTESIAN_POINT('Ctrl Pts',(19.2054070165995,-0.626173010563829,
3.97108838428485));
#17691=CARTESIAN_POINT('Ctrl Pts',(19.1895017379119,-0.59622098845213,4.19351757937831));
#17692=CARTESIAN_POINT('Ctrl Pts',(19.1735964592243,-0.479600048885993,
4.35228505390253));
#17693=CARTESIAN_POINT('Ctrl Pts',(19.1586794432354,-0.370225264934164,
4.50118762911129));
#17694=CARTESIAN_POINT('Ctrl Pts',(19.1437624272465,-0.184617181632464,
4.59409385471947));
#17695=CARTESIAN_POINT('Ctrl Pts',(19.1288454112575,0.000222628893785728,
4.59497983522242));
#17696=CARTESIAN_POINT('Ctrl Pts',(19.0211545887425,-0.000526118841417405,
4.59432346427954));
#17697=CARTESIAN_POINT('Ctrl Pts',(19.0242658457596,-0.0391895592568775,
4.59468017342281));
#17698=CARTESIAN_POINT('Ctrl Pts',(19.0273771027768,-0.0777896429211806,
4.59123148246997));
#17699=CARTESIAN_POINT('Ctrl Pts',(19.030488359794,-0.115590453236054,4.58374636034569));
#17700=CARTESIAN_POINT('Ctrl Pts',(19.0463936384816,-0.308834669113126,
4.5454811341878));
#17701=CARTESIAN_POINT('Ctrl Pts',(19.0622989171692,-0.481190439544719,
4.40172662532195));
#17702=CARTESIAN_POINT('Ctrl Pts',(19.0782041958568,-0.553519286527586,
4.21848882245705));
#17703=CARTESIAN_POINT('Ctrl Pts',(19.0941094745444,-0.625848133510457,
4.03525101959215));
#17704=CARTESIAN_POINT('Ctrl Pts',(19.1100147532321,-0.598150057044591,
3.81252992272818));
#17705=CARTESIAN_POINT('Ctrl Pts',(19.1259200319197,-0.483142842019737,
3.65258963701249));
#17706=CARTESIAN_POINT('Ctrl Pts',(19.1418253106073,-0.36813562699489,3.49264935129682));
#17707=CARTESIAN_POINT('Ctrl Pts',(19.1577305892949,-0.165819273411065,
3.39548987672941));
#17708=CARTESIAN_POINT('Ctrl Pts',(19.1736358679825,0.0309111084379188,
3.40572273351557));
#17709=CARTESIAN_POINT('Ctrl Pts',(19.1895411466701,0.227641490286902,3.41595559030173));
#17710=CARTESIAN_POINT('Ctrl Pts',(19.2054464253577,0.418785900401045,3.53358077844144));
#17711=CARTESIAN_POINT('Ctrl Pts',(19.2213517040453,0.516578912360374,3.70458978792342));
#17712=CARTESIAN_POINT('Ctrl Pts',(19.237256982733,0.614371924319703,3.87559879740541));
#17713=CARTESIAN_POINT('Ctrl Pts',(19.2531622614206,0.618813538124218,4.09999162822965));
#17714=CARTESIAN_POINT('Ctrl Pts',(19.2690675401082,0.527864352527146,4.27473658562515));
#17715=CARTESIAN_POINT('Ctrl Pts',(19.2849728187958,0.436915166930073,4.44948154302064));
#17716=CARTESIAN_POINT('Ctrl Pts',(19.3008780974834,0.250575181931413,4.5745786269874));
#17717=CARTESIAN_POINT('Ctrl Pts',(19.316783376171,0.0544038354309166,4.59258854924263));
#17718=CARTESIAN_POINT('Ctrl Pts',(19.3182404470282,0.0364327229714708,
4.59423842494573));
#17719=CARTESIAN_POINT('Ctrl Pts',(19.3196975178853,0.0183791031991185,
4.59498959766064));
#17720=CARTESIAN_POINT('Ctrl Pts',(19.3211545887425,0.000315695961457875,
4.59487351203822));
#17721=CARTESIAN_POINT('Origin',(4.,0.,4.));
#17722=CARTESIAN_POINT('',(19.7288454112575,-0.000401422265437046,4.59340756962635));
#17723=CARTESIAN_POINT('',(19.6211545887425,0.000364945106097663,4.59334757974602));
#17724=CARTESIAN_POINT('',(4.,-7.27562663373442E-17,4.5941));
#17725=CARTESIAN_POINT('Ctrl Pts',(19.7288454112575,-0.000401422265437046,
4.59340756962635));
#17726=CARTESIAN_POINT('Ctrl Pts',(19.7187204928102,0.125914276337785,4.59262579220321));
#17727=CARTESIAN_POINT('Ctrl Pts',(19.7085955743629,0.252675872983383,4.55317429478549));
#17728=CARTESIAN_POINT('Ctrl Pts',(19.6984706559155,0.353547469597214,4.47867015725961));
#17729=CARTESIAN_POINT('Ctrl Pts',(19.6825653772279,0.512007102052776,4.36163128164859));
#17730=CARTESIAN_POINT('Ctrl Pts',(19.6666600985403,0.606576931433326,4.15809158444534));
#17731=CARTESIAN_POINT('Ctrl Pts',(19.6507548198527,0.593834428727047,3.9615078130365));
#17732=CARTESIAN_POINT('Ctrl Pts',(19.6348495411651,0.581091926020768,3.76492404162769));
#17733=CARTESIAN_POINT('Ctrl Pts',(19.6189442624775,0.46103709122769,3.57529619601327));
#17734=CARTESIAN_POINT('Ctrl Pts',(19.6030389837899,0.288794059426421,3.47969339775167));
#17735=CARTESIAN_POINT('Ctrl Pts',(19.5871337051022,0.116551027625133,3.38409059949006));
#17736=CARTESIAN_POINT('Ctrl Pts',(19.5712284264146,-0.107880201184358,
3.38251284858128));
#17737=CARTESIAN_POINT('Ctrl Pts',(19.555323147727,-0.281450319664219,3.47568456171554));
#17738=CARTESIAN_POINT('Ctrl Pts',(19.5394178690394,-0.45502043814407,3.5688562748498));
#17739=CARTESIAN_POINT('Ctrl Pts',(19.5235125903518,-0.577729446294298,
3.75677745202708));
#17740=CARTESIAN_POINT('Ctrl Pts',(19.5076073116642,-0.593234549413986,
3.95316264945144));
#17741=CARTESIAN_POINT('Ctrl Pts',(19.4917020329766,-0.608739652533674,
4.1495478468758));
#17742=CARTESIAN_POINT('Ctrl Pts',(19.475796754289,-0.517040850622822,4.35439706454724));
#17743=CARTESIAN_POINT('Ctrl Pts',(19.4598914756013,-0.360242359119356,
4.47365220261941));
#17744=CARTESIAN_POINT('Ctrl Pts',(19.4495427874867,-0.258222223711561,
4.55124494740629));
#17745=CARTESIAN_POINT('Ctrl Pts',(19.4391940993721,-0.128642866595325,
4.59260240088276));
#17746=CARTESIAN_POINT('Ctrl Pts',(19.4288454112575,0.000431836873498515,
4.59346738712276));
#17747=CARTESIAN_POINT('Ctrl Pts',(19.3211545887425,0.000315695961457875,
4.59487351203822));
#17748=CARTESIAN_POINT('Ctrl Pts',(19.3356027965729,-0.178799726336078,
4.59372241551416));
#17749=CARTESIAN_POINT('Ctrl Pts',(19.3500510044034,-0.35887750705714,4.50729762043595));
#17750=CARTESIAN_POINT('Ctrl Pts',(19.3644992122339,-0.469016560662847,
4.36625733020606));
#17751=CARTESIAN_POINT('Ctrl Pts',(19.3804044909215,-0.590262902253753,
4.21099342837053));
#17752=CARTESIAN_POINT('Ctrl Pts',(19.3963097696091,-0.626752877433238,
3.98954286415574));
#17753=CARTESIAN_POINT('Ctrl Pts',(19.4122150482967,-0.561731832709929,
3.80358636875254));
#17754=CARTESIAN_POINT('Ctrl Pts',(19.4281203269843,-0.49671078798662,3.61762987334934));
#17755=CARTESIAN_POINT('Ctrl Pts',(19.4440256056719,-0.330178723360516,
3.46716744675772));
#17756=CARTESIAN_POINT('Ctrl Pts',(19.4599308843595,-0.138600118749324,
3.42128506802099));
#17757=CARTESIAN_POINT('Ctrl Pts',(19.4758361630471,0.0529784858618673,
3.37540268928427));
#17758=CARTESIAN_POINT('Ctrl Pts',(19.4917414417347,0.269603630458146,3.43410035840244));
#17759=CARTESIAN_POINT('Ctrl Pts',(19.5076467204224,0.411810215621333,3.57042659223364));
#17760=CARTESIAN_POINT('Ctrl Pts',(19.52355199911,0.554016800784528,3.70675282606484));
#17761=CARTESIAN_POINT('Ctrl Pts',(19.5394572777976,0.621804826514621,3.92070762460909));
#17762=CARTESIAN_POINT('Ctrl Pts',(19.5553625564852,0.584048894878601,4.11405198996909));
#17763=CARTESIAN_POINT('Ctrl Pts',(19.5712678351728,0.546292963242583,4.30739635532907));
#17764=CARTESIAN_POINT('Ctrl Pts',(19.5871731138604,0.402993074240464,4.4801302875048));
#17765=CARTESIAN_POINT('Ctrl Pts',(19.6030783925481,0.219946482677819,4.55294168410437));
#17766=CARTESIAN_POINT('Ctrl Pts',(19.6091037912795,0.150602919307179,4.5805248346624));
#17767=CARTESIAN_POINT('Ctrl Pts',(19.615129190011,0.0755552166468998,4.59376787586841));
#17768=CARTESIAN_POINT('Ctrl Pts',(19.6211545887425,0.000364945106097663,
4.59334757974602));
#17769=CARTESIAN_POINT('Origin',(4.,0.,4.));
#17770=CARTESIAN_POINT('',(20.0288454112575,-0.000266600559035268,4.5949350414008));
#17771=CARTESIAN_POINT('',(19.9211545887425,-0.000461335262921832,4.59353843444423));
#17772=CARTESIAN_POINT('',(4.,-7.27562663373442E-17,4.5941));
#17773=CARTESIAN_POINT('Ctrl Pts',(20.0288454112575,-0.000266600559035268,
4.5949350414008));
#17774=CARTESIAN_POINT('Ctrl Pts',(20.0141521649359,0.181839152323842,4.59391190659116));
#17775=CARTESIAN_POINT('Ctrl Pts',(19.9994589186142,0.364814066967773,4.50413264800542));
#17776=CARTESIAN_POINT('Ctrl Pts',(19.9847656722925,0.474598868642052,4.35899217880197));
#17777=CARTESIAN_POINT('Ctrl Pts',(19.9688603936049,0.593439717564554,4.20187920587587));
#17778=CARTESIAN_POINT('Ctrl Pts',(19.9529551149173,0.626517665065843,3.97989492921597));
#17779=CARTESIAN_POINT('Ctrl Pts',(19.9370498362297,0.558641803885684,3.79496194153783));
#17780=CARTESIAN_POINT('Ctrl Pts',(19.9211445575421,0.490765942705524,3.61002895385969));
#17781=CARTESIAN_POINT('Ctrl Pts',(19.9052392788545,0.321936272843916,3.46214725516331));
#17782=CARTESIAN_POINT('Ctrl Pts',(19.8893340001669,0.129673778938228,3.41921955761011));
#17783=CARTESIAN_POINT('Ctrl Pts',(19.8734287214793,-0.0625887149674591,
3.37629186005692));
#17784=CARTESIAN_POINT('Ctrl Pts',(19.8575234427916,-0.278284032917226,
3.43831816364691));
#17785=CARTESIAN_POINT('Ctrl Pts',(19.841618164104,-0.418374827314372,3.57681771754473));
#17786=CARTESIAN_POINT('Ctrl Pts',(19.8257128854164,-0.558465621711518,
3.71531727144255));
#17787=CARTESIAN_POINT('Ctrl Pts',(19.8098076067288,-0.622951892556044,
3.9302900756482));
#17788=CARTESIAN_POINT('Ctrl Pts',(19.7939023280412,-0.58222383973146,4.12303018792675));
#17789=CARTESIAN_POINT('Ctrl Pts',(19.7779970493536,-0.541495786906873,
4.3157703002053));
#17790=CARTESIAN_POINT('Ctrl Pts',(19.762091770666,-0.395553410413165,4.48627772055676));
#17791=CARTESIAN_POINT('Ctrl Pts',(19.7461864919784,-0.211407504401025,
4.55626240372308));
#17792=CARTESIAN_POINT('Ctrl Pts',(19.7404061317381,-0.144484459893097,
4.58169651826758));
#17793=CARTESIAN_POINT('Ctrl Pts',(19.7346257714978,-0.0725156072563085,
4.59385388977766));
#17794=CARTESIAN_POINT('Ctrl Pts',(19.7288454112575,-0.000401422265437046,
4.59340756962635));
#17795=CARTESIAN_POINT('Ctrl Pts',(19.6211545887425,0.000364945106097663,
4.59334757974602));
#17796=CARTESIAN_POINT('Ctrl Pts',(19.6310344686986,-0.122924963130536,
4.59265841784648));
#17797=CARTESIAN_POINT('Ctrl Pts',(19.6409143486547,-0.246598186964828,
4.55523353708024));
#17798=CARTESIAN_POINT('Ctrl Pts',(19.6507942286109,-0.346136160298313,
4.48405653351353));
#17799=CARTESIAN_POINT('Ctrl Pts',(19.6666995072985,-0.506378917588675,
4.36947112529969));
#17800=CARTESIAN_POINT('Ctrl Pts',(19.6826047859861,-0.60407113804621,4.16741144784858));
#17801=CARTESIAN_POINT('Ctrl Pts',(19.6985100646737,-0.5943566574826,3.97065479758251));
#17802=CARTESIAN_POINT('Ctrl Pts',(19.7144153433613,-0.584642176918989,
3.77389814731645));
#17803=CARTESIAN_POINT('Ctrl Pts',(19.7303206220489,-0.467520995334232,
3.58244452423543));
#17804=CARTESIAN_POINT('Ctrl Pts',(19.7462259007365,-0.296770260159971,
3.48420125495101));
#17805=CARTESIAN_POINT('Ctrl Pts',(19.7621311794242,-0.12601952498572,3.38595798566659));
#17806=CARTESIAN_POINT('Ctrl Pts',(19.7780364581118,0.098360763778029,3.38092507017875));
#17807=CARTESIAN_POINT('Ctrl Pts',(19.7939417367994,0.27334477570878,3.47141355644931));
#17808=CARTESIAN_POINT('Ctrl Pts',(19.809847015487,0.448328787639532,3.56190204271987));
#17809=CARTESIAN_POINT('Ctrl Pts',(19.8257522941746,0.573916522737285,3.74791193074883));
#17810=CARTESIAN_POINT('Ctrl Pts',(19.8416575728622,0.592443207149574,3.9440350735258));
#17811=CARTESIAN_POINT('Ctrl Pts',(19.8575628515498,0.610969891561863,4.14015821630277));
#17812=CARTESIAN_POINT('Ctrl Pts',(19.8734681302375,0.522435525288687,4.34639461382776));
#17813=CARTESIAN_POINT('Ctrl Pts',(19.8893734089251,0.367491719635661,4.46804975837363));
#17814=CARTESIAN_POINT('Ctrl Pts',(19.8999671355309,0.264291244586565,4.54907828775811));
#17815=CARTESIAN_POINT('Ctrl Pts',(19.9105608621367,0.131629953687138,4.59258455010229));
#17816=CARTESIAN_POINT('Ctrl Pts',(19.9211545887425,-0.000461335262921832,
4.59353843444423));
#17817=CARTESIAN_POINT('Origin',(4.,0.,4.));
#17818=CARTESIAN_POINT('',(20.3288454112575,0.000547175593784699,4.59423670486774));
#17819=CARTESIAN_POINT('',(20.2211545887425,-0.000159442692484791,4.59503650419094));
#17820=CARTESIAN_POINT('',(4.,-7.27562663373442E-17,4.5941));
#17821=CARTESIAN_POINT('Ctrl Pts',(20.3288454112575,0.000547175593784699,
4.59423670486774));
#17822=CARTESIAN_POINT('Ctrl Pts',(20.3254891157492,0.0422991098545892,
4.59465405164581));
#17823=CARTESIAN_POINT('Ctrl Pts',(20.3221328202408,0.0839734681026259,
4.59066114403672));
#17824=CARTESIAN_POINT('Ctrl Pts',(20.3187765247324,0.124636177719752,4.58197547152207));
#17825=CARTESIAN_POINT('Ctrl Pts',(20.3028712460448,0.317334266145104,4.54081460186972));
#17826=CARTESIAN_POINT('Ctrl Pts',(20.2869659673572,0.48731321493246,4.39426577643889));
#17827=CARTESIAN_POINT('Ctrl Pts',(20.2710606886696,0.556778600406793,4.20989870881916));
#17828=CARTESIAN_POINT('Ctrl Pts',(20.255155409982,0.626243985881127,4.02553164119943));
#17829=CARTESIAN_POINT('Ctrl Pts',(20.2392501312944,0.595195808042437,3.80334633139079));
#17830=CARTESIAN_POINT('Ctrl Pts',(20.2233448526068,0.477757630702126,3.64521515909767));
#17831=CARTESIAN_POINT('Ctrl Pts',(20.2074395739191,0.360319453361808,3.48708398680455));
#17832=CARTESIAN_POINT('Ctrl Pts',(20.1915342952315,0.156491276519859,3.39300695202695));
#17833=CARTESIAN_POINT('Ctrl Pts',(20.1756290165439,-0.04006765138094,3.40625706061923));
#17834=CARTESIAN_POINT('Ctrl Pts',(20.1597237378563,-0.236626579281727,
3.4195071692115));
#17835=CARTESIAN_POINT('Ctrl Pts',(20.1438184591687,-0.425916258241364,
3.54008442117362));
#17836=CARTESIAN_POINT('Ctrl Pts',(20.1279131804811,-0.521059912873915,
3.71258420787224));
#17837=CARTESIAN_POINT('Ctrl Pts',(20.1120079017935,-0.616203567506467,
3.88508399457085));
#17838=CARTESIAN_POINT('Ctrl Pts',(20.0961026231058,-0.617201197811932,
4.10950631600596));
#17839=CARTESIAN_POINT('Ctrl Pts',(20.0801973444182,-0.523575121773085,
4.28282745216878));
#17840=CARTESIAN_POINT('Ctrl Pts',(20.0642920657306,-0.429949045734243,
4.45614858833159));
#17841=CARTESIAN_POINT('Ctrl Pts',(20.048386787043,-0.241699263351099,4.57836853922213));
#17842=CARTESIAN_POINT('Ctrl Pts',(20.0324815083554,-0.0452724969876719,
4.59335768007126));
#17843=CARTESIAN_POINT('Ctrl Pts',(20.0312694759895,-0.030304158296608,
4.59449989984645));
#17844=CARTESIAN_POINT('Ctrl Pts',(20.0300574436235,-0.0152883365109376,
4.5950194388496));
#17845=CARTESIAN_POINT('Ctrl Pts',(20.0288454112575,-0.000266600559035268,
4.5949350414008));
#17846=CARTESIAN_POINT('Ctrl Pts',(19.9211545887425,-0.000461335262921832,
4.59353843444423));
#17847=CARTESIAN_POINT('Ctrl Pts',(19.9264661408243,-0.0666901315043342,
4.5940166992278));
#17848=CARTESIAN_POINT('Ctrl Pts',(19.9317776929061,-0.132775635823809,
4.58379778651276));
#17849=CARTESIAN_POINT('Ctrl Pts',(19.9370892449879,-0.194932679790098,
4.56224768701753));
#17850=CARTESIAN_POINT('Ctrl Pts',(19.9529945236755,-0.381060028529917,
4.49771657954882));
#17851=CARTESIAN_POINT('Ctrl Pts',(19.9688998023631,-0.531961480976676,
4.33158047304464));
#17852=CARTESIAN_POINT('Ctrl Pts',(19.9848050810507,-0.578348134104426,
4.14012389605102));
#17853=CARTESIAN_POINT('Ctrl Pts',(20.0007103597384,-0.624734787232175,
3.94866731905739));
#17854=CARTESIAN_POINT('Ctrl Pts',(20.016615638426,-0.566606641040915,3.73189027157431));
#17855=CARTESIAN_POINT('Ctrl Pts',(20.0325209171136,-0.430656211588969,
3.58932409618151));
#17856=CARTESIAN_POINT('Ctrl Pts',(20.0484261958012,-0.294705782137024,
3.44675792078871));
#17857=CARTESIAN_POINT('Ctrl Pts',(20.0643314744888,-0.080933069424392,
3.37840261748619));
#17858=CARTESIAN_POINT('Ctrl Pts',(20.0802367531764,0.112511319004002,3.41565067076361));
#17859=CARTESIAN_POINT('Ctrl Pts',(20.096142031864,0.305955707432406,3.45289872404102));
#17860=CARTESIAN_POINT('Ctrl Pts',(20.1120473105516,0.479071771576571,3.59575013389837));
#17861=CARTESIAN_POINT('Ctrl Pts',(20.1279525892393,0.552362916535151,3.77860107435498));
#17862=CARTESIAN_POINT('Ctrl Pts',(20.1438578679269,0.625654061493722,3.96145201481158));
#17863=CARTESIAN_POINT('Ctrl Pts',(20.1597631466145,0.599120287266732,4.18430248586742));
#17864=CARTESIAN_POINT('Ctrl Pts',(20.1756684253021,0.484961816589866,4.3448525870839));
#17865=CARTESIAN_POINT('Ctrl Pts',(20.1908304797822,0.376137759761604,4.49790047950022));
#17866=CARTESIAN_POINT('Ctrl Pts',(20.2059925342623,0.187686755696174,4.59433432972249));
#17867=CARTESIAN_POINT('Ctrl Pts',(20.2211545887425,-0.000159442692484791,
4.59503650419094));
#17868=CARTESIAN_POINT('Origin',(4.,0.,4.));
#17869=CARTESIAN_POINT('',(20.6288454112575,1.84392275237588E-6,4.59415158619139));
#17870=CARTESIAN_POINT('',(20.5211545887425,0.00014515264107467,4.59408556636595));
#17871=CARTESIAN_POINT('',(4.,-7.27562663373442E-17,4.5941));
#17872=CARTESIAN_POINT('Ctrl Pts',(20.6288454112575,1.84392275237588E-6,
4.59415158619139));
#17873=CARTESIAN_POINT('Ctrl Pts',(20.6209207878748,0.0985777406598016,
4.59414764832452));
#17874=CARTESIAN_POINT('Ctrl Pts',(20.6129961644921,0.197149291092008,4.56908802213256));
#17875=CARTESIAN_POINT('Ctrl Pts',(20.6050715411094,0.283761277174982,4.52200793915563));
#17876=CARTESIAN_POINT('Ctrl Pts',(20.5971189017656,0.370679463050262,4.47476141372331));
#17877=CARTESIAN_POINT('Ctrl Pts',(20.5891662624218,0.445553373684486,4.40533845822152));
#17878=CARTESIAN_POINT('Ctrl Pts',(20.581213623078,0.499196468040806,4.3222224876916));
#17879=CARTESIAN_POINT('Ctrl Pts',(20.5732609837342,0.552839562397126,4.23910651716169));
#17880=CARTESIAN_POINT('Ctrl Pts',(20.5653083443904,0.585251840475543,4.14229753160364));
#17881=CARTESIAN_POINT('Ctrl Pts',(20.5573557050466,0.592531230276538,4.04364021904617));
#17882=CARTESIAN_POINT('Ctrl Pts',(20.5494030657028,0.599810620077534,3.9449829064887));
#17883=CARTESIAN_POINT('Ctrl Pts',(20.541450426359,0.581957121601108,3.84447726693182));
#17884=CARTESIAN_POINT('Ctrl Pts',(20.5334977870152,0.541038843355354,3.75439549632807));
#17885=CARTESIAN_POINT('Ctrl Pts',(20.5255451476714,0.5001205651096,3.66431372572433));
#17886=CARTESIAN_POINT('Ctrl Pts',(20.5175925083276,0.436137507094518,3.58465582407373));
#17887=CARTESIAN_POINT('Ctrl Pts',(20.5096398689838,0.357128912623608,3.5251911792601));
#17888=CARTESIAN_POINT('Ctrl Pts',(20.50168722964,0.278120318152698,3.46572653444646));
#17889=CARTESIAN_POINT('Ctrl Pts',(20.4937345902962,0.184086187225959,3.42645514646979));
#17890=CARTESIAN_POINT('Ctrl Pts',(20.4857819509524,0.0861162623359374,
3.4121221101222));
#17891=CARTESIAN_POINT('Ctrl Pts',(20.4778293116085,-0.0118536625540841,
3.39778907377461));
#17892=CARTESIAN_POINT('Ctrl Pts',(20.4698766722647,-0.113759381407388,
3.4083943890561));
#17893=CARTESIAN_POINT('Ctrl Pts',(20.4619240329209,-0.206384677702653,
3.44274365129583));
#17894=CARTESIAN_POINT('Ctrl Pts',(20.4539713935771,-0.299009973997917,
3.47709291353557));
#17895=CARTESIAN_POINT('Ctrl Pts',(20.4460187542333,-0.382354847735142,
3.53518612273354));
#17896=CARTESIAN_POINT('Ctrl Pts',(20.4380661148895,-0.447563842371028,
3.60976099223211));
#17897=CARTESIAN_POINT('Ctrl Pts',(20.4301134755457,-0.512772837006921,
3.68433586173069));
#17898=CARTESIAN_POINT('Ctrl Pts',(20.4221608362019,-0.559845952541473,
3.77539239152987));
#17899=CARTESIAN_POINT('Ctrl Pts',(20.4142081968581,-0.580888308445953,
3.87190852591559));
#17900=CARTESIAN_POINT('Ctrl Pts',(20.3983029181705,-0.622973020254908,
4.06494079468701));
#17901=CARTESIAN_POINT('Ctrl Pts',(20.3823976394829,-0.5609346935436,4.27981148180459));
#17902=CARTESIAN_POINT('Ctrl Pts',(20.3664923607953,-0.422206916156273,
4.41936036842645));
#17903=CARTESIAN_POINT('Ctrl Pts',(20.353943377616,-0.312753156865475,4.52946196836027));
#17904=CARTESIAN_POINT('Ctrl Pts',(20.3413943944368,-0.155560747392339,
4.59267627084609));
#17905=CARTESIAN_POINT('Ctrl Pts',(20.3288454112575,0.000547175593784699,
4.59423670486774));
#17906=CARTESIAN_POINT('Ctrl Pts',(20.2211545887425,-0.000159442692484791,
4.59503650419094));
#17907=CARTESIAN_POINT('Ctrl Pts',(20.22189781295,-0.00936741923094289,
4.59507092387091));
#17908=CARTESIAN_POINT('Ctrl Pts',(20.2226410371574,-0.0185739425223631,
4.59487531632137));
#17909=CARTESIAN_POINT('Ctrl Pts',(20.2233842613649,-0.0277695625699301,
4.59444507412072));
#17910=CARTESIAN_POINT('Ctrl Pts',(20.2392895400526,-0.224559303926058,
4.58523772856393));
#17911=CARTESIAN_POINT('Ctrl Pts',(20.2551948187402,-0.416355619511548,
4.46857330607325));
#17912=CARTESIAN_POINT('Ctrl Pts',(20.2711000974278,-0.51503297954037,4.29810345018796));
#17913=CARTESIAN_POINT('Ctrl Pts',(20.2870053761154,-0.613710339569191,
4.12763359430267));
#17914=CARTESIAN_POINT('Ctrl Pts',(20.302910654803,-0.619268744041345,3.90335830502277));
#17915=CARTESIAN_POINT('Ctrl Pts',(20.3188159334906,-0.529271009537506,
3.72809546473432));
#17916=CARTESIAN_POINT('Ctrl Pts',(20.3347212121782,-0.439273275033663,
3.55283262444587));
#17917=CARTESIAN_POINT('Ctrl Pts',(20.3506264908658,-0.253719401553817,
3.42658223314887));
#17918=CARTESIAN_POINT('Ctrl Pts',(20.3665317695535,-0.0575887485100287,
3.40762076142476));
#17919=CARTESIAN_POINT('Ctrl Pts',(20.3824370482411,0.138541904533748,3.38865928970065));
#17920=CARTESIAN_POINT('Ctrl Pts',(20.3983423269287,0.345249337141466,3.47698673754941));
#17921=CARTESIAN_POINT('Ctrl Pts',(20.4142476056163,0.467192899405167,3.63141813202173));
#17922=CARTESIAN_POINT('Ctrl Pts',(20.4301528843039,0.589136461668875,3.78584952649406));
#17923=CARTESIAN_POINT('Ctrl Pts',(20.4460581629915,0.626316153588557,4.00638486758996));
#17924=CARTESIAN_POINT('Ctrl Pts',(20.4619634416791,0.562534942182983,4.19337293359078));
#17925=CARTESIAN_POINT('Ctrl Pts',(20.4699160810229,0.530644336480201,4.28686696659118));
#17926=CARTESIAN_POINT('Ctrl Pts',(20.4778687203667,0.473513504946115,4.3719741808178));
#17927=CARTESIAN_POINT('Ctrl Pts',(20.4858213597105,0.400240502138227,4.43864269813793));
#17928=CARTESIAN_POINT('Ctrl Pts',(20.4937739990544,0.326967499330329,4.50531121545807));
#17929=CARTESIAN_POINT('Ctrl Pts',(20.5017266383982,0.237552325248626,4.55354103587171));
#17930=CARTESIAN_POINT('Ctrl Pts',(20.509679277742,0.141619450488441,4.57712494713439));
#17931=CARTESIAN_POINT('Ctrl Pts',(20.5135043814088,0.0954771353210092,
4.58846846487098));
#17932=CARTESIAN_POINT('Ctrl Pts',(20.5173294850756,0.0478269697500401,
4.59411022582368));
#17933=CARTESIAN_POINT('Ctrl Pts',(20.5211545887425,0.00014515264107467,
4.59408556636595));
#17934=CARTESIAN_POINT('Origin',(4.,0.,4.));
#17935=CARTESIAN_POINT('',(20.9288454112575,-6.4040329070536E-6,4.59405282094147));
#17936=CARTESIAN_POINT('',(20.8211545887425,5.65245430726296E-6,4.59414685459231));
#17937=CARTESIAN_POINT('',(4.,-7.27562663373442E-17,4.5941));
#17938=CARTESIAN_POINT('Ctrl Pts',(20.9288454112575,-6.4040329070536E-6,
4.59405282094147));
#17939=CARTESIAN_POINT('Ctrl Pts',(20.9243050993443,0.0564994875152707,
4.59403151438501));
#17940=CARTESIAN_POINT('Ctrl Pts',(20.9197647874311,0.113011285737041,4.58603249222448));
#17941=CARTESIAN_POINT('Ctrl Pts',(20.9152244755179,0.167207550221224,4.57013805289591));
#17942=CARTESIAN_POINT('Ctrl Pts',(20.9072718361741,0.262135685878584,4.5422979516059));
#17943=CARTESIAN_POINT('Ctrl Pts',(20.8993191968303,0.349959832061366,4.49023494241839));
#17944=CARTESIAN_POINT('Ctrl Pts',(20.8913665574865,0.419942299057043,4.42031443844746));
#17945=CARTESIAN_POINT('Ctrl Pts',(20.8834139181427,0.489924766052721,4.35039393447653));
#17946=CARTESIAN_POINT('Ctrl Pts',(20.8754612787989,0.542065553861293,4.26261593572219));
#17947=CARTESIAN_POINT('Ctrl Pts',(20.8675086394551,0.569989725359365,4.16771249585991));
#17948=CARTESIAN_POINT('Ctrl Pts',(20.8595560001113,0.597913896857441,4.07280905599763));
#17949=CARTESIAN_POINT('Ctrl Pts',(20.8516033607674,0.601621452045013,3.97078017502742));
#17950=CARTESIAN_POINT('Ctrl Pts',(20.8436507214236,0.580659121393648,3.87410027737825));
#17951=CARTESIAN_POINT('Ctrl Pts',(20.8356980820798,0.559696790742287,3.77742037972911));
#17952=CARTESIAN_POINT('Ctrl Pts',(20.827745442736,0.514064574252002,3.686089465401));
#17953=CARTESIAN_POINT('Ctrl Pts',(20.8197928033922,0.44934157601673,3.61127397478397));
#17954=CARTESIAN_POINT('Ctrl Pts',(20.8118401640484,0.384618577781443,3.53645848416692));
#17955=CARTESIAN_POINT('Ctrl Pts',(20.8038875247046,0.300804797801161,3.47815841726095));
#17956=CARTESIAN_POINT('Ctrl Pts',(20.7959348853608,0.208147717693743,3.44350176598286));
#17957=CARTESIAN_POINT('Ctrl Pts',(20.787982246017,0.115490637586335,3.40884511470477));
#17958=CARTESIAN_POINT('Ctrl Pts',(20.7800296066732,0.0139902573517945,
3.39783187905454));
#17959=CARTESIAN_POINT('Ctrl Pts',(20.7720769673294,-0.0839438183138644,
3.41180854931868));
#17960=CARTESIAN_POINT('Ctrl Pts',(20.7641243279856,-0.181877893979523,
3.42578521958283));
#17961=CARTESIAN_POINT('Ctrl Pts',(20.7561716886418,-0.2762456650763,3.46475179576135));
#17962=CARTESIAN_POINT('Ctrl Pts',(20.748219049298,-0.355509010203556,3.52394413563581));
#17963=CARTESIAN_POINT('Ctrl Pts',(20.7402664099542,-0.434772355330821,
3.58313647551028));
#17964=CARTESIAN_POINT('Ctrl Pts',(20.7323137706103,-0.498931274488562,
3.66255457908069));
#17965=CARTESIAN_POINT('Ctrl Pts',(20.7243611312665,-0.54014217617541,3.75248840252759));
#17966=CARTESIAN_POINT('Ctrl Pts',(20.7164084919227,-0.581353077862249,
3.84242222597448));
#17967=CARTESIAN_POINT('Ctrl Pts',(20.7084558525789,-0.599615962078206,
3.94287176929784));
#17968=CARTESIAN_POINT('Ctrl Pts',(20.7005032132351,-0.592696601504336,
4.0415558946729));
#17969=CARTESIAN_POINT('Ctrl Pts',(20.6925505738913,-0.585777240930466,
4.14024002004797));
#17970=CARTESIAN_POINT('Ctrl Pts',(20.6845979345475,-0.553675635566762,
4.23715872747472));
#17971=CARTESIAN_POINT('Ctrl Pts',(20.6766452952037,-0.50031917594212,4.32046203197985));
#17972=CARTESIAN_POINT('Ctrl Pts',(20.6686926558599,-0.446962716317479,
4.40376533648498));
#17973=CARTESIAN_POINT('Ctrl Pts',(20.6607400165161,-0.3723514024319,4.47345323806848));
#17974=CARTESIAN_POINT('Ctrl Pts',(20.6527873771723,-0.285602702553558,
4.52100610813718));
#17975=CARTESIAN_POINT('Ctrl Pts',(20.6448347378285,-0.198854002675205,
4.56855897820588));
#17976=CARTESIAN_POINT('Ctrl Pts',(20.6368820984847,-0.099967916804087,
4.59397681675976));
#17977=CARTESIAN_POINT('Ctrl Pts',(20.6289294591409,-0.00104364331035449,
4.59415068835528));
#17978=CARTESIAN_POINT('Ctrl Pts',(20.6289014431798,-0.000695147863829354,
4.59415130087895));
#17979=CARTESIAN_POINT('Ctrl Pts',(20.6288734272186,-0.000346651943377611,
4.59415160011295));
#17980=CARTESIAN_POINT('Ctrl Pts',(20.6288454112575,1.84392275237588E-6,
4.59415158619139));
#17981=CARTESIAN_POINT('Ctrl Pts',(20.5211545887425,0.00014515264107467,
4.59408556636595));
#17982=CARTESIAN_POINT('Ctrl Pts',(20.5252821244194,-0.0513066296901884,
4.59405895720698));
#17983=CARTESIAN_POINT('Ctrl Pts',(20.5294096600964,-0.102795266482965,
4.58743447362686));
#17984=CARTESIAN_POINT('Ctrl Pts',(20.5335371957734,-0.152465997634008,
4.57425651377355));
#17985=CARTESIAN_POINT('Ctrl Pts',(20.5414898351172,-0.248167995557571,
4.5488661670383));
#17986=CARTESIAN_POINT('Ctrl Pts',(20.549442474461,-0.33712141596603,4.49914747145609));
#17987=CARTESIAN_POINT('Ctrl Pts',(20.5573951138048,-0.408848640915227,
4.43107686705031));
#17988=CARTESIAN_POINT('Ctrl Pts',(20.5653477531486,-0.480575865864423,
4.36300626264453));
#17989=CARTESIAN_POINT('Ctrl Pts',(20.5733003924924,-0.535076895354358,
4.27658374941519));
#17990=CARTESIAN_POINT('Ctrl Pts',(20.5812530318362,-0.565476628275392,
4.18243021985824));
#17991=CARTESIAN_POINT('Ctrl Pts',(20.58920567118,-0.595876361196427,4.08827669030129));
#17992=CARTESIAN_POINT('Ctrl Pts',(20.5971583105238,-0.602174797548561,
3.98639214441672));
#17993=CARTESIAN_POINT('Ctrl Pts',(20.6051109498677,-0.58371402745925,3.88920441471463));
#17994=CARTESIAN_POINT('Ctrl Pts',(20.6130635892115,-0.565253257369939,
3.79201668501254));
#17995=CARTESIAN_POINT('Ctrl Pts',(20.6210162285553,-0.522033280839182,
3.69952577149293));
#17996=CARTESIAN_POINT('Ctrl Pts',(20.6289688678991,-0.459278917219465,
3.62305528060961));
#17997=CARTESIAN_POINT('Ctrl Pts',(20.6369215072429,-0.396524553599749,
3.54658478972629));
#17998=CARTESIAN_POINT('Ctrl Pts',(20.6448741465867,-0.314235802891072,
3.48613472147926));
#17999=CARTESIAN_POINT('Ctrl Pts',(20.6528267859305,-0.222505051509483,
3.44908779917463));
#18000=CARTESIAN_POINT('Ctrl Pts',(20.6607794252743,-0.130774300127894,
3.41204087687));
#18001=CARTESIAN_POINT('Ctrl Pts',(20.6687320646181,-0.029601548073392,
3.39839710050778));
#18002=CARTESIAN_POINT('Ctrl Pts',(20.6766847039619,0.0686601223983595,
3.40982890848785));
#18003=CARTESIAN_POINT('Ctrl Pts',(20.6846373433057,0.1669217928701,3.42126071646792));
#18004=CARTESIAN_POINT('Ctrl Pts',(20.6925899826495,0.262272381759091,3.45776810879028));
#18005=CARTESIAN_POINT('Ctrl Pts',(20.7005426219933,0.343045155251024,3.51488528173127));
#18006=CARTESIAN_POINT('Ctrl Pts',(20.7084952613371,0.423817928742975,3.57200245467228));
#18007=CARTESIAN_POINT('Ctrl Pts',(20.7164479006809,0.490012886837861,3.64972940823193));
#18008=CARTESIAN_POINT('Ctrl Pts',(20.7244005400247,0.533541468465666,3.73856417004634));
#18009=CARTESIAN_POINT('Ctrl Pts',(20.7323531793686,0.577070050093471,3.82739893186076));
#18010=CARTESIAN_POINT('Ctrl Pts',(20.7403058187123,0.597932255254196,3.92734150192994));
#18011=CARTESIAN_POINT('Ctrl Pts',(20.7482584580562,0.593574919799613,4.02617190099588));
#18012=CARTESIAN_POINT('Ctrl Pts',(20.7562110974,0.589217584345031,4.1250023000618));
#18013=CARTESIAN_POINT('Ctrl Pts',(20.7641637367438,0.559640708275147,4.22272052812447));
#18014=CARTESIAN_POINT('Ctrl Pts',(20.7721163760876,0.508461778515953,4.30737953925928));
#18015=CARTESIAN_POINT('Ctrl Pts',(20.7800690154314,0.457282848756759,4.39203855039408));
#18016=CARTESIAN_POINT('Ctrl Pts',(20.7880216547752,0.384501865308254,4.46363834460102));
#18017=CARTESIAN_POINT('Ctrl Pts',(20.795974294119,0.299016600344635,4.51342469267633));
#18018=CARTESIAN_POINT('Ctrl Pts',(20.8039269334628,0.213531335381016,4.56321104075164));
#18019=CARTESIAN_POINT('Ctrl Pts',(20.8118795728066,0.115341788902283,4.59118394269532));
#18020=CARTESIAN_POINT('Ctrl Pts',(20.8198322121504,0.0164533379892873,
4.59392342516246));
#18021=CARTESIAN_POINT('Ctrl Pts',(20.8202730043478,0.0109722321971217,
4.59407526688998));
#18022=CARTESIAN_POINT('Ctrl Pts',(20.8207137965451,0.00548897925183007,
4.59414958726715));
#18023=CARTESIAN_POINT('Ctrl Pts',(20.8211545887425,5.65245430726296E-6,
4.59414685459231));
#18024=CARTESIAN_POINT('Origin',(4.,0.,4.));
#18025=CARTESIAN_POINT('',(21.2288454112575,1.28243205298473E-5,4.59412621697841));
#18026=CARTESIAN_POINT('',(21.1211545887425,-1.09306879613159E-5,4.5940621922514));
#18027=CARTESIAN_POINT('',(4.,-7.27562663373442E-17,4.5941));
#18028=CARTESIAN_POINT('Ctrl Pts',(21.2288454112575,1.28243205298473E-5,
4.59412621697841));
#18029=CARTESIAN_POINT('Ctrl Pts',(21.2276894108138,0.0143945780386088,
4.59413985249388));
#18030=CARTESIAN_POINT('Ctrl Pts',(21.2265334103701,0.028775363636007,4.59362827285675));
#18031=CARTESIAN_POINT('Ctrl Pts',(21.2253774099263,0.043117441953227,4.59258471957415));
#18032=CARTESIAN_POINT('Ctrl Pts',(21.2174247705826,0.141782954511012,4.58540565408365));
#18033=CARTESIAN_POINT('Ctrl Pts',(21.2094721312387,0.238616577754522,4.55305001116024));
#18034=CARTESIAN_POINT('Ctrl Pts',(21.2015194918949,0.321779082392626,4.49947370882601));
#18035=CARTESIAN_POINT('Ctrl Pts',(21.1935668525511,0.404941587030731,4.44589740649178));
#18036=CARTESIAN_POINT('Ctrl Pts',(21.1856142132073,0.474432973063433,4.37110044474674));
#18037=CARTESIAN_POINT('Ctrl Pts',(21.1776615738635,0.521756972098598,4.28422777087894));
#18038=CARTESIAN_POINT('Ctrl Pts',(21.1697089345197,0.569080971133768,4.19735509701114));
#18039=CARTESIAN_POINT('Ctrl Pts',(21.1617562951759,0.594237583171398,4.09840671102057));
#18040=CARTESIAN_POINT('Ctrl Pts',(21.1538036558321,0.594151069756079,3.9994804007435));
#18041=CARTESIAN_POINT('Ctrl Pts',(21.1458510164883,0.59406455634076,3.90055409046644));
#18042=CARTESIAN_POINT('Ctrl Pts',(21.1378983771445,0.568734917472505,3.80164985590287));
#18043=CARTESIAN_POINT('Ctrl Pts',(21.1299457378007,0.521259046500119,3.71486008677882));
#18044=CARTESIAN_POINT('Ctrl Pts',(21.1219930984569,0.473783175527722,3.62807031765475));
#18045=CARTESIAN_POINT('Ctrl Pts',(21.114040459113,0.40416107245118,3.5533950139702));
#18046=CARTESIAN_POINT('Ctrl Pts',(21.1060878197692,0.320904987578411,3.49996424865404));
#18047=CARTESIAN_POINT('Ctrl Pts',(21.0981351804254,0.237648902705652,3.44653348333788));
#18048=CARTESIAN_POINT('Ctrl Pts',(21.0901825410817,0.140758836036697,3.41434725639011));
#18049=CARTESIAN_POINT('Ctrl Pts',(21.0822299017378,0.042080917889342,3.40734077242984));
#18050=CARTESIAN_POINT('Ctrl Pts',(21.074277262394,-0.056597000258024,3.40033428846957));
#18051=CARTESIAN_POINT('Ctrl Pts',(21.0663246230502,-0.157062769883762,
3.41850754749682));
#18052=CARTESIAN_POINT('Ctrl Pts',(21.0583719837064,-0.247033082431791,
3.45963862106718));
#18053=CARTESIAN_POINT('Ctrl Pts',(21.0504193443626,-0.337003394979799,
3.50076969463752));
#18054=CARTESIAN_POINT('Ctrl Pts',(21.0424667050188,-0.416478250450111,
3.56485858275095));
#18055=CARTESIAN_POINT('Ctrl Pts',(21.034514065675,-0.475740765152555,3.644069545988));
#18056=CARTESIAN_POINT('Ctrl Pts',(21.0265614263312,-0.535003279855012,
3.72328050922507));
#18057=CARTESIAN_POINT('Ctrl Pts',(21.0186087869874,-0.574053453789596,
3.81761354758578));
#18058=CARTESIAN_POINT('Ctrl Pts',(21.0106561476436,-0.588116871685884,
3.91553516229212));
#18059=CARTESIAN_POINT('Ctrl Pts',(21.0027035082998,-0.60218028958217,4.01345677699845));
#18060=CARTESIAN_POINT('Ctrl Pts',(20.994750868956,-0.591256951440166,4.11496696805043));
#18061=CARTESIAN_POINT('Ctrl Pts',(20.9867982296121,-0.556682383467722,
4.20765473214191));
#18062=CARTESIAN_POINT('Ctrl Pts',(20.9788455902683,-0.522107815495282,
4.30034249623339));
#18063=CARTESIAN_POINT('Ctrl Pts',(20.9708929509246,-0.463882017692404,
4.38420783336438));
#18064=CARTESIAN_POINT('Ctrl Pts',(20.9629403115808,-0.389123888092725,
4.4489970636758));
#18065=CARTESIAN_POINT('Ctrl Pts',(20.9549876722369,-0.314365758493028,
4.51378629398723));
#18066=CARTESIAN_POINT('Ctrl Pts',(20.9470350328931,-0.223075297096518,
4.5594994174791));
#18067=CARTESIAN_POINT('Ctrl Pts',(20.9390823935493,-0.12641400383229,4.58054738252877));
#18068=CARTESIAN_POINT('Ctrl Pts',(20.9356700661187,-0.0849384674446181,
4.58957866703598));
#18069=CARTESIAN_POINT('Ctrl Pts',(20.9322577386881,-0.0424741039190781,
4.59406883414683));
#18070=CARTESIAN_POINT('Ctrl Pts',(20.9288454112575,-6.4040329070536E-6,
4.59405282094147));
#18071=CARTESIAN_POINT('Ctrl Pts',(20.8211545887425,5.65245430726296E-6,
4.59414685459231));
#18072=CARTESIAN_POINT('Ctrl Pts',(20.8286664358889,-0.0934395423672534,
4.59410028517524));
#18073=CARTESIAN_POINT('Ctrl Pts',(20.8361782830354,-0.18690618531264,4.57167601133058));
#18074=CARTESIAN_POINT('Ctrl Pts',(20.8436901301818,-0.270133012248912,
4.529191754035));
#18075=CARTESIAN_POINT('Ctrl Pts',(20.8516427695256,-0.358243556226857,
4.4842145374498));
#18076=CARTESIAN_POINT('Ctrl Pts',(20.8595954088694,-0.434877288835492,
4.41675404128879));
#18077=CARTESIAN_POINT('Ctrl Pts',(20.8675480482133,-0.490664589397756,
4.33505825661903));
#18078=CARTESIAN_POINT('Ctrl Pts',(20.8755006875571,-0.546451889960021,
4.25336247194927));
#18079=CARTESIAN_POINT('Ctrl Pts',(20.8834533269009,-0.581392758475918,
4.15743139877076));
#18080=CARTESIAN_POINT('Ctrl Pts',(20.8914059662447,-0.591215252505097,
4.05899390323763));
#18081=CARTESIAN_POINT('Ctrl Pts',(20.8993586055885,-0.601037746534278,
3.96055640770449));
#18082=CARTESIAN_POINT('Ctrl Pts',(20.9073112449323,-0.585741866076735,
3.85961248981672));
#18083=CARTESIAN_POINT('Ctrl Pts',(20.9152638842761,-0.547197711916726,
3.76850392583047));
#18084=CARTESIAN_POINT('Ctrl Pts',(20.9232165236199,-0.508653557756717,
3.67739536184422));
#18085=CARTESIAN_POINT('Ctrl Pts',(20.9311691629637,-0.446861129894262,
3.59612215175949));
#18086=CARTESIAN_POINT('Ctrl Pts',(20.9391218023075,-0.369375409551539,
3.53462104847409));
#18087=CARTESIAN_POINT('Ctrl Pts',(20.9470744416513,-0.291889689208826,
3.4731199451887));
#18088=CARTESIAN_POINT('Ctrl Pts',(20.9550270809951,-0.198710676385865,
3.43139094870266));
#18089=CARTESIAN_POINT('Ctrl Pts',(20.9629797203389,-0.101230766359376,
3.41453599926792));
#18090=CARTESIAN_POINT('Ctrl Pts',(20.9709323596827,-0.00375085633288601,
3.39768104983318));
#18091=CARTESIAN_POINT('Ctrl Pts',(20.9788849990265,0.0980299508971346,
3.40570014744973));
#18092=CARTESIAN_POINT('Ctrl Pts',(20.9868376383704,0.191667561123074,3.43761284710704));
#18093=CARTESIAN_POINT('Ctrl Pts',(20.9947902777142,0.285305171349014,3.46952554676435));
#18094=CARTESIAN_POINT('Ctrl Pts',(21.002742917058,0.37079958457088,3.52533184846243));
#18095=CARTESIAN_POINT('Ctrl Pts',(21.0106955564018,0.437697946637459,3.59820867233944));
#18096=CARTESIAN_POINT('Ctrl Pts',(21.0186481957456,0.504596308704037,3.67108549621644));
#18097=CARTESIAN_POINT('Ctrl Pts',(21.0266008350894,0.552898619615334,3.76103284227238));
#18098=CARTESIAN_POINT('Ctrl Pts',(21.0345534744332,0.576699262792956,3.8570534220826));
#18099=CARTESIAN_POINT('Ctrl Pts',(21.042506113777,0.600499905970578,3.95307400189282));
#18100=CARTESIAN_POINT('Ctrl Pts',(21.0504587531208,0.599798881414527,4.05516781545734));
#18101=CARTESIAN_POINT('Ctrl Pts',(21.0584113924646,0.574681899562831,4.15085250374278));
#18102=CARTESIAN_POINT('Ctrl Pts',(21.0663640318084,0.549564917711138,4.24653719202821));
#18103=CARTESIAN_POINT('Ctrl Pts',(21.0743166711522,0.500031978563804,4.33581275503458));
#18104=CARTESIAN_POINT('Ctrl Pts',(21.082269310496,0.432139158218639,4.40776403918836));
#18105=CARTESIAN_POINT('Ctrl Pts',(21.0902219498398,0.364246337873458,4.47971532334216));
#18106=CARTESIAN_POINT('Ctrl Pts',(21.0981745891836,0.277993636330433,4.53434232864337));
#18107=CARTESIAN_POINT('Ctrl Pts',(21.1061272285274,0.183926621270441,4.56496615973523));
#18108=CARTESIAN_POINT('Ctrl Pts',(21.1111363485991,0.124676735433976,4.5842551580617));
#18109=CARTESIAN_POINT('Ctrl Pts',(21.1161454686708,0.0623266393968894,
4.59402126159141));
#18110=CARTESIAN_POINT('Ctrl Pts',(21.1211545887425,-1.09306879613159E-5,
4.5940621922514));
#18111=CARTESIAN_POINT('Origin',(4.,0.,4.));
#18112=CARTESIAN_POINT('',(21.5288454112575,-1.51073027558624E-5,4.59408477831653));
#18113=CARTESIAN_POINT('',(21.4211545887425,1.51733402061755E-5,4.59410821609125));
#18114=CARTESIAN_POINT('',(4.,-7.27562663373442E-17,4.5941));
#18115=CARTESIAN_POINT('Ctrl Pts',(21.5288454112575,-1.51073027558624E-5,
4.59408477831653));
#18116=CARTESIAN_POINT('Ctrl Pts',(21.5231210829395,0.0712153309254728,
4.59401644885886));
#18117=CARTESIAN_POINT('Ctrl Pts',(21.5173967546214,0.142469702059594,4.58119587380047));
#18118=CARTESIAN_POINT('Ctrl Pts',(21.5116724263034,0.209120766622247,4.55613331912479));
#18119=CARTESIAN_POINT('Ctrl Pts',(21.5037197869596,0.301717111362981,4.52131465616629));
#18120=CARTESIAN_POINT('Ctrl Pts',(21.4957671476158,0.385428743083265,4.46286809139133));
#18121=CARTESIAN_POINT('Ctrl Pts',(21.4878145082719,0.450020774675764,4.38793951336988));
#18122=CARTESIAN_POINT('Ctrl Pts',(21.4798618689281,0.514612806268249,4.31301093534845));
#18123=CARTESIAN_POINT('Ctrl Pts',(21.4719092295843,0.560085237732952,4.22160034408054));
#18124=CARTESIAN_POINT('Ctrl Pts',(21.4639565902405,0.58087844500124,4.1248839293359));
#18125=CARTESIAN_POINT('Ctrl Pts',(21.4560039508967,0.601671652269532,4.02816751459124));
#18126=CARTESIAN_POINT('Ctrl Pts',(21.4480513115529,0.597785635341394,3.92614527636987));
#18127=CARTESIAN_POINT('Ctrl Pts',(21.4400986722091,0.569695512712777,3.83129082280931));
#18128=CARTESIAN_POINT('Ctrl Pts',(21.4321460328653,0.541605390084162,3.73643636924876));
#18129=CARTESIAN_POINT('Ctrl Pts',(21.4241933935215,0.489311161755075,3.64874970034904));
#18130=CARTESIAN_POINT('Ctrl Pts',(21.4162407541777,0.419206509371839,3.57895170565158));
#18131=CARTESIAN_POINT('Ctrl Pts',(21.4082881148339,0.349101856988603,3.50915371095413));
#18132=CARTESIAN_POINT('Ctrl Pts',(21.4003354754901,0.261186780551223,3.45724439045894));
#18133=CARTESIAN_POINT('Ctrl Pts',(21.3923828361463,0.16621009553345,3.42957036558731));
#18134=CARTESIAN_POINT('Ctrl Pts',(21.3844301968025,0.0712334105156764,
3.40189634071567));
#18135=CARTESIAN_POINT('Ctrl Pts',(21.3764775574587,-0.0308048830825163,
3.3984576114676));
#18136=CARTESIAN_POINT('Ctrl Pts',(21.3685249181149,-0.127429214135013,
3.41967460932821));
#18137=CARTESIAN_POINT('Ctrl Pts',(21.360572278771,-0.22405354518751,3.44089160718882));
#18138=CARTESIAN_POINT('Ctrl Pts',(21.3526196394272,-0.315263913694308,
3.4867643321581));
#18139=CARTESIAN_POINT('Ctrl Pts',(21.3446670000834,-0.389908609845283,
3.5516842188346));
#18140=CARTESIAN_POINT('Ctrl Pts',(21.3367143607396,-0.464553305996249,
3.6166041055111));
#18141=CARTESIAN_POINT('Ctrl Pts',(21.3287617213958,-0.522632329791381,
3.70057115389483));
#18142=CARTESIAN_POINT('Ctrl Pts',(21.320809082052,-0.557044729551177,3.79331924871262));
#18143=CARTESIAN_POINT('Ctrl Pts',(21.3128564427082,-0.591457129310977,
3.88606734353042));
#18144=CARTESIAN_POINT('Ctrl Pts',(21.3049038033644,-0.602202905035458,
3.9875964847823));
#18145=CARTESIAN_POINT('Ctrl Pts',(21.2969511640206,-0.587968239287942,
4.08549335215105));
#18146=CARTESIAN_POINT('Ctrl Pts',(21.2889985246768,-0.573733573540424,
4.18339021951981));
#18147=CARTESIAN_POINT('Ctrl Pts',(21.281045885333,-0.534518466320906,4.27765481300544));
#18148=CARTESIAN_POINT('Ctrl Pts',(21.2730932459892,-0.47511749858569,4.35676200219639));
#18149=CARTESIAN_POINT('Ctrl Pts',(21.2651406066454,-0.415716530850488,
4.43586919138732));
#18150=CARTESIAN_POINT('Ctrl Pts',(21.2571879673016,-0.336129702599601,
4.49981897628356));
#18151=CARTESIAN_POINT('Ctrl Pts',(21.2492353279577,-0.246087587538132,
4.54079262470289));
#18152=CARTESIAN_POINT('Ctrl Pts',(21.2424386890577,-0.169134048541188,
4.57581031891556));
#18153=CARTESIAN_POINT('Ctrl Pts',(21.2356420501576,-0.0845438791841879,
4.59404604774026));
#18154=CARTESIAN_POINT('Ctrl Pts',(21.2288454112575,1.28243205298473E-5,
4.59412621697841));
#18155=CARTESIAN_POINT('Ctrl Pts',(21.1211545887425,-1.09306879613159E-5,
4.5940621922514));
#18156=CARTESIAN_POINT('Ctrl Pts',(21.1240981080146,-0.0366424819978743,
4.5940862444172));
#18157=CARTESIAN_POINT('Ctrl Pts',(21.1270416272867,-0.0732697079540161,
4.59075208378119));
#18158=CARTESIAN_POINT('Ctrl Pts',(21.1299851465589,-0.109260984540888,
4.58401866488291));
#18159=CARTESIAN_POINT('Ctrl Pts',(21.1379377859027,-0.20650024671525,4.56582668205621));
#18160=CARTESIAN_POINT('Ctrl Pts',(21.1458904252465,-0.299097442487026,
4.52282205952027));
#18161=CARTESIAN_POINT('Ctrl Pts',(21.1538430645903,-0.375731303474415,
4.46026269810429));
#18162=CARTESIAN_POINT('Ctrl Pts',(21.1617957039341,-0.452365164461805,
4.3977033366883));
#18163=CARTESIAN_POINT('Ctrl Pts',(21.1697483432779,-0.513035690664809,
4.31558923639226));
#18164=CARTESIAN_POINT('Ctrl Pts',(21.1777009826217,-0.550325083965727,
4.22395996434209));
#18165=CARTESIAN_POINT('Ctrl Pts',(21.1856536219655,-0.587614477266646,
4.13233069229192));
#18166=CARTESIAN_POINT('Ctrl Pts',(21.1936062613093,-0.601522737665479,
4.03118624848761));
#18167=CARTESIAN_POINT('Ctrl Pts',(21.2015589006531,-0.590349390887683,
3.93289291874755));
#18168=CARTESIAN_POINT('Ctrl Pts',(21.2095115399969,-0.579176044109886,
3.83459958900749));
#18169=CARTESIAN_POINT('Ctrl Pts',(21.2174641793407,-0.542921090155459,
3.73915737333167));
#18170=CARTESIAN_POINT('Ctrl Pts',(21.2254168186845,-0.486017190935348,
3.65823538248142));
#18171=CARTESIAN_POINT('Ctrl Pts',(21.2333694580283,-0.429113291715238,
3.57731339163117));
#18172=CARTESIAN_POINT('Ctrl Pts',(21.2413220973721,-0.351560447229444,
3.51091162560648));
#18173=CARTESIAN_POINT('Ctrl Pts',(21.249274736716,-0.262840548960938,3.46714860467879));
#18174=CARTESIAN_POINT('Ctrl Pts',(21.2572273760598,-0.174120650692433,
3.4233855837511));
#18175=CARTESIAN_POINT('Ctrl Pts',(21.2651800154036,-0.0742336986412151,
3.40226130792041));
#18176=CARTESIAN_POINT('Ctrl Pts',(21.2731326547474,0.0246077668693877,
3.40635850761334));
#18177=CARTESIAN_POINT('Ctrl Pts',(21.2810852940912,0.123449232380002,3.41045570730627));
#18178=CARTESIAN_POINT('Ctrl Pts',(21.289037933435,0.221245211350001,3.43977438252282));
#18179=CARTESIAN_POINT('Ctrl Pts',(21.2969905727788,0.306038813396919,3.49072992590572));
#18180=CARTESIAN_POINT('Ctrl Pts',(21.3049432121226,0.390832415443818,3.54168546928862));
#18181=CARTESIAN_POINT('Ctrl Pts',(21.3128958514664,0.462623640567642,3.61427788083785));
#18182=CARTESIAN_POINT('Ctrl Pts',(21.3208484908102,0.512635033719562,3.69963174955258));
#18183=CARTESIAN_POINT('Ctrl Pts',(21.328801130154,0.562646426871494,3.78498561826733));
#18184=CARTESIAN_POINT('Ctrl Pts',(21.3367537694978,0.590877988051513,3.88310094414759));
#18185=CARTESIAN_POINT('Ctrl Pts',(21.3447064088416,0.59387802439953,3.98198179230066));
#18186=CARTESIAN_POINT('Ctrl Pts',(21.3526590481854,0.596878060747546,4.08086264045372));
#18187=CARTESIAN_POINT('Ctrl Pts',(21.3606116875293,0.574646572263566,4.1805090108796));
#18188=CARTESIAN_POINT('Ctrl Pts',(21.3685643268731,0.529901661201384,4.26873777763737));
#18189=CARTESIAN_POINT('Ctrl Pts',(21.3765169662169,0.485156750139203,4.35696654439514));
#18190=CARTESIAN_POINT('Ctrl Pts',(21.3844696055607,0.417898416498819,4.4337777074848));
#18191=CARTESIAN_POINT('Ctrl Pts',(21.3924222449045,0.336349907607971,4.48978005607163));
#18192=CARTESIAN_POINT('Ctrl Pts',(21.4003748842483,0.254801398717122,4.54578240465847));
#18193=CARTESIAN_POINT('Ctrl Pts',(21.4083275235921,0.158962714575808,4.58097593874246));
#18194=CARTESIAN_POINT('Ctrl Pts',(21.4162801629359,0.0605514396169286,
4.59105776945554));
#18195=CARTESIAN_POINT('Ctrl Pts',(21.4179049715381,0.0404449719157324,
4.59311759444699));
#18196=CARTESIAN_POINT('Ctrl Pts',(21.4195297801403,0.0202311170044278,
4.59412918598148));
#18197=CARTESIAN_POINT('Ctrl Pts',(21.4211545887425,1.51733402061755E-5,
4.59410821609125));
#18198=CARTESIAN_POINT('Origin',(4.,0.,4.));
#18199=CARTESIAN_POINT('',(21.8288454112575,1.47252919898561E-5,4.59408074293421));
#18200=CARTESIAN_POINT('',(21.7211545887425,-1.54601956517634E-5,4.59410286710644));
#18201=CARTESIAN_POINT('',(4.,-7.27562663373442E-17,4.5941));
#18202=CARTESIAN_POINT('Ctrl Pts',(21.8288454112575,1.47252919898561E-5,
4.59408074293421));
#18203=CARTESIAN_POINT('Ctrl Pts',(21.826505394409,0.0291331941223908,4.59410767674242));
#18204=CARTESIAN_POINT('Ctrl Pts',(21.8241653775604,0.0582478076928112,
4.59200528777341));
#18205=CARTESIAN_POINT('Ctrl Pts',(21.8218253607118,0.0870422430987805,
4.58774093918134));
#18206=CARTESIAN_POINT('Ctrl Pts',(21.813872721368,0.184901264939656,4.57324838268129));
#18207=CARTESIAN_POINT('Ctrl Pts',(21.8059200820242,0.279062206656402,4.53378504179028));
#18208=CARTESIAN_POINT('Ctrl Pts',(21.7979674426804,0.358012610677869,4.47417584741217));
#18209=CARTESIAN_POINT('Ctrl Pts',(21.7900148033366,0.436963014699336,4.41456665303406));
#18210=CARTESIAN_POINT('Ctrl Pts',(21.7820621639928,0.500702881025523,4.33481160516884));
#18211=CARTESIAN_POINT('Ctrl Pts',(21.774109524649,0.541439142878506,4.24466184465998));
#18212=CARTESIAN_POINT('Ctrl Pts',(21.7661568853052,0.58217540473149,4.15451208415111));
#18213=CARTESIAN_POINT('Ctrl Pts',(21.7582042459614,0.599908062111268,4.0539676109986));
#18214=CARTESIAN_POINT('Ctrl Pts',(21.7502516066176,0.59246905613922,3.95532135643358));
#18215=CARTESIAN_POINT('Ctrl Pts',(21.7422989672738,0.585030050167171,3.85667510186855));
#18216=CARTESIAN_POINT('Ctrl Pts',(21.73434632793,0.552419380843296,3.759927065891));
#18217=CARTESIAN_POINT('Ctrl Pts',(21.7263936885861,0.498624146640836,3.67690601358098));
#18218=CARTESIAN_POINT('Ctrl Pts',(21.7184410492423,0.444828912438376,3.59388496127097));
#18219=CARTESIAN_POINT('Ctrl Pts',(21.7104884098985,0.369849113357332,3.52459089262848));
#18220=CARTESIAN_POINT('Ctrl Pts',(21.7025357705547,0.28285205103972,3.47749595131133));
#18221=CARTESIAN_POINT('Ctrl Pts',(21.6945831312109,0.195854988722108,3.43040100999418));
#18222=CARTESIAN_POINT('Ctrl Pts',(21.6866304918671,0.0968406631679286,
3.40550519600236));
#18223=CARTESIAN_POINT('Ctrl Pts',(21.6786778525233,-0.00208507577578169,
3.40585236167057));
#18224=CARTESIAN_POINT('Ctrl Pts',(21.6707252131795,-0.101010814719503,
3.40619952733877));
#18225=CARTESIAN_POINT('Ctrl Pts',(21.6627725738357,-0.199847967052756,
3.431789672667));
#18226=CARTESIAN_POINT('Ctrl Pts',(21.6548199344919,-0.28651234476781,3.47949405385809));
#18227=CARTESIAN_POINT('Ctrl Pts',(21.6468672951481,-0.373176722482865,
3.52719843504918));
#18228=CARTESIAN_POINT('Ctrl Pts',(21.6389146558043,-0.44766832557972,3.59701705210314));
#18229=CARTESIAN_POINT('Ctrl Pts',(21.6309620164605,-0.500879541024521,
3.68041362817464));
#18230=CARTESIAN_POINT('Ctrl Pts',(21.6230093771167,-0.55409075646931,3.76381020424612));
#18231=CARTESIAN_POINT('Ctrl Pts',(21.6150567377728,-0.586021584262053,
3.86078473933514));
#18232=CARTESIAN_POINT('Ctrl Pts',(21.607104098429,-0.592768045815946,3.95948077576042));
#18233=CARTESIAN_POINT('Ctrl Pts',(21.5991514590852,-0.599514507369841,
4.05817681218572));
#18234=CARTESIAN_POINT('Ctrl Pts',(21.5911988197414,-0.581076602684875,
4.15859434994728));
#18235=CARTESIAN_POINT('Ctrl Pts',(21.5832461803976,-0.539708616728004,
4.24845597739434));
#18236=CARTESIAN_POINT('Ctrl Pts',(21.5752935410538,-0.498340630771147,
4.33831760484137));
#18237=CARTESIAN_POINT('Ctrl Pts',(21.56734090171,-0.434042563542403,4.41762332197391));
#18238=CARTESIAN_POINT('Ctrl Pts',(21.5593882623662,-0.354675729482573,
4.47667692475034));
#18239=CARTESIAN_POINT('Ctrl Pts',(21.5514356230224,-0.275308895422716,
4.53573052752678));
#18240=CARTESIAN_POINT('Ctrl Pts',(21.5434829836786,-0.180873294531764,
4.57453201594709));
#18241=CARTESIAN_POINT('Ctrl Pts',(21.5355303443348,-0.0829149652056982,
4.58833737958621));
#18242=CARTESIAN_POINT('Ctrl Pts',(21.533302033309,-0.055467269432644,4.59220561033096));
#18243=CARTESIAN_POINT('Ctrl Pts',(21.5310737222833,-0.0277430016607059,
4.5941113769453));
#18244=CARTESIAN_POINT('Ctrl Pts',(21.5288454112575,-1.51073027558624E-5,
4.59408477831653));
#18245=CARTESIAN_POINT('Ctrl Pts',(21.4211545887425,1.51733402061755E-5,
4.59410821609125));
#18246=CARTESIAN_POINT('Ctrl Pts',(21.4274824194841,-0.0787159889745399,
4.59402654867773));
#18247=CARTESIAN_POINT('Ctrl Pts',(21.4338102502257,-0.15747883181342,4.57828382012605));
#18248=CARTESIAN_POINT('Ctrl Pts',(21.4401380809673,-0.230053504748576,
4.54780575811717));
#18249=CARTESIAN_POINT('Ctrl Pts',(21.4480907203111,-0.321263308378747,
4.50950178872359));
#18250=CARTESIAN_POINT('Ctrl Pts',(21.4560433596549,-0.402699049862651,
4.44792372259427));
#18251=CARTESIAN_POINT('Ctrl Pts',(21.4639959989987,-0.464404100671371,
4.37060031698995));
#18252=CARTESIAN_POINT('Ctrl Pts',(21.4719486383425,-0.526109151480106,
4.2932769113856));
#18253=CARTESIAN_POINT('Ctrl Pts',(21.4799012776864,-0.568083511613643,
4.20020816630624));
#18254=CARTESIAN_POINT('Ctrl Pts',(21.4878539170302,-0.585195243866348,
4.10277300340868));
#18255=CARTESIAN_POINT('Ctrl Pts',(21.495806556374,-0.602306976119048,4.00533784051114));
#18256=CARTESIAN_POINT('Ctrl Pts',(21.5037591957178,-0.594556080490919,
3.90353625979537));
#18257=CARTESIAN_POINT('Ctrl Pts',(21.5117118350616,-0.562890209537588,
3.80981489101362));
#18258=CARTESIAN_POINT('Ctrl Pts',(21.5196644744054,-0.53122433858425,3.71609352223184));
#18259=CARTESIAN_POINT('Ctrl Pts',(21.5276171137492,-0.47564349230572,3.63045236538409));
#18260=CARTESIAN_POINT('Ctrl Pts',(21.535569753093,-0.402943186155437,3.56336221830407));
#18261=CARTESIAN_POINT('Ctrl Pts',(21.5435223924368,-0.330242880005154,
3.49627207122406));
#18262=CARTESIAN_POINT('Ctrl Pts',(21.5514750317806,-0.24042311398314,3.44773293391182));
#18263=CARTESIAN_POINT('Ctrl Pts',(21.5594276711244,-0.144465577806233,
3.42367937699355));
#18264=CARTESIAN_POINT('Ctrl Pts',(21.5673803104682,-0.0485080416293372,
3.39962582007528));
#18265=CARTESIAN_POINT('Ctrl Pts',(21.575332949812,0.0535872647024426,3.40005784355098));
#18266=CARTESIAN_POINT('Ctrl Pts',(21.5832855891558,0.149337799479898,3.42492262666669));
#18267=CARTESIAN_POINT('Ctrl Pts',(21.5912382284996,0.245088334257342,3.44978740978241));
#18268=CARTESIAN_POINT('Ctrl Pts',(21.5991908678434,0.33449409748049,3.49908495253815));
#18269=CARTESIAN_POINT('Ctrl Pts',(21.6071435071872,0.406624016913212,3.56678795891296));
#18270=CARTESIAN_POINT('Ctrl Pts',(21.6150961465311,0.478753936345942,3.63449096528778));
#18271=CARTESIAN_POINT('Ctrl Pts',(21.6230487858749,0.533608011988269,3.72059943528167));
#18272=CARTESIAN_POINT('Ctrl Pts',(21.6310014252187,0.564479585995414,3.81458543566408));
#18273=CARTESIAN_POINT('Ctrl Pts',(21.6389540645625,0.595351160002559,3.90857143604649));
#18274=CARTESIAN_POINT('Ctrl Pts',(21.6469067039063,0.602240232374519,4.0104349668174));
#18275=CARTESIAN_POINT('Ctrl Pts',(21.6548593432501,0.584304520186539,4.10772182398666));
#18276=CARTESIAN_POINT('Ctrl Pts',(21.6628119825939,0.566368807998562,4.2050086811559));
#18277=CARTESIAN_POINT('Ctrl Pts',(21.6707646219377,0.523608311250652,4.29771886472347));
#18278=CARTESIAN_POINT('Ctrl Pts',(21.6787172612815,0.461251083056512,4.37451729206089));
#18279=CARTESIAN_POINT('Ctrl Pts',(21.6866699006253,0.398893854862358,4.45131571939834));
#18280=CARTESIAN_POINT('Ctrl Pts',(21.6946225399691,0.316939895221968,4.51220239050563));
#18281=CARTESIAN_POINT('Ctrl Pts',(21.7025751793129,0.225409191891896,4.54973308058009));
#18282=CARTESIAN_POINT('Ctrl Pts',(21.7087683157894,0.15412944274098,4.5789601931952));
#18283=CARTESIAN_POINT('Ctrl Pts',(21.7149614522659,0.0770418275534371,
4.59402294959611));
#18284=CARTESIAN_POINT('Ctrl Pts',(21.7211545887425,-1.54601956517634E-5,
4.59410286710644));
#18285=CARTESIAN_POINT('Origin',(4.,0.,4.));
#18286=CARTESIAN_POINT('',(22.1288454112575,-1.19684274697274E-5,4.59413016891312));
#18287=CARTESIAN_POINT('',(22.0211545887425,1.20066176157995E-5,4.59406577061205));
#18288=CARTESIAN_POINT('',(4.,-7.27562663373442E-17,4.5941));
#18289=CARTESIAN_POINT('Ctrl Pts',(22.1288454112575,-1.19684274697274E-5,
4.59413016891312));
#18290=CARTESIAN_POINT('Ctrl Pts',(22.1219370665346,0.0859328098890183,
4.59405244111828));
#18291=CARTESIAN_POINT('Ctrl Pts',(22.1150287218117,0.171910584533005,4.57519344187135));
#18292=CARTESIAN_POINT('Ctrl Pts',(22.1081203770888,0.24987714748571,4.53905210772026));
#18293=CARTESIAN_POINT('Ctrl Pts',(22.100167737745,0.339629466009183,4.49744749656716));
#18294=CARTESIAN_POINT('Ctrl Pts',(22.0922150984012,0.418765494330909,4.4329406966096));
#18295=CARTESIAN_POINT('Ctrl Pts',(22.0842624590574,0.477609775176754,4.35341854270704));
#18296=CARTESIAN_POINT('Ctrl Pts',(22.0763098197136,0.536454056022584,4.2738963888045));
#18297=CARTESIAN_POINT('Ctrl Pts',(22.0683571803698,0.575006589392542,4.17935888095698));
#18298=CARTESIAN_POINT('Ctrl Pts',(22.060404541026,0.588553803007579,4.081364517074));
#18299=CARTESIAN_POINT('Ctrl Pts',(22.0524519016822,0.60210101662262,3.983370153191));
#18300=CARTESIAN_POINT('Ctrl Pts',(22.0444992623384,0.590642910482727,3.88191893327255));
#18301=CARTESIAN_POINT('Ctrl Pts',(22.0365466229946,0.55558039411957,3.78941465069146));
#18302=CARTESIAN_POINT('Ctrl Pts',(22.0285939836508,0.520517877756421,3.69691036811039));
#18303=CARTESIAN_POINT('Ctrl Pts',(22.020641344307,0.461850951170019,3.61335302286667));
#18304=CARTESIAN_POINT('Ctrl Pts',(22.0126887049632,0.386752445163155,3.5489586384446));
#18305=CARTESIAN_POINT('Ctrl Pts',(22.0047360656194,0.311653939156274,3.48456425402251));
#18306=CARTESIAN_POINT('Ctrl Pts',(21.9967834262756,0.220123853728924,3.43933283042207));
#18307=CARTESIAN_POINT('Ctrl Pts',(21.9888307869318,0.123352988439278,3.41879452521803));
#18308=CARTESIAN_POINT('Ctrl Pts',(21.980878147588,0.0265821231496428,3.398256220014));
#18309=CARTESIAN_POINT('Ctrl Pts',(21.9729255082441,-0.075429522002288,
3.40241103320635));
#18310=CARTESIAN_POINT('Ctrl Pts',(21.9649728689003,-0.170209634025949,
3.43075098229493));
#18311=CARTESIAN_POINT('Ctrl Pts',(21.9570202295565,-0.26498974604961,3.4590909313835));
#18312=CARTESIAN_POINT('Ctrl Pts',(21.9490675902127,-0.352538324945002,
3.5116160163683));
#18313=CARTESIAN_POINT('Ctrl Pts',(21.9411149508689,-0.422151364554475,
3.58190433023263));
#18314=CARTESIAN_POINT('Ctrl Pts',(21.9331623115251,-0.491764404163956,
3.65219264409696));
#18315=CARTESIAN_POINT('Ctrl Pts',(21.9252096721813,-0.543441904487514,
3.74024418684083));
#18316=CARTESIAN_POINT('Ctrl Pts',(21.9172570328375,-0.570865587277161,
3.83529345812586));
#18317=CARTESIAN_POINT('Ctrl Pts',(21.9093043934937,-0.598289270066803,
3.93034272941087));
#18318=CARTESIAN_POINT('Ctrl Pts',(21.9013517541499,-0.601459135322544,
4.03238972923704));
#18319=CARTESIAN_POINT('Ctrl Pts',(21.8933991148061,-0.579987623844179,
4.12895782202339));
#18320=CARTESIAN_POINT('Ctrl Pts',(21.8854464754623,-0.558516112365809,
4.22552591480976));
#18321=CARTESIAN_POINT('Ctrl Pts',(21.8774938361185,-0.512403224153321,
4.31661510055631));
#18322=CARTESIAN_POINT('Ctrl Pts',(21.8695411967747,-0.447286887835617,
4.39108848569571));
#18323=CARTESIAN_POINT('Ctrl Pts',(21.8615885574308,-0.38217055151792,4.46556187083511));
#18324=CARTESIAN_POINT('Ctrl Pts',(21.853635918087,-0.298050767095013,4.52341945536736));
#18325=CARTESIAN_POINT('Ctrl Pts',(21.8456832787432,-0.205212323901057,
4.55758736157894));
#18326=CARTESIAN_POINT('Ctrl Pts',(21.840070656248,-0.139691040693493,4.58170156451555));
#18327=CARTESIAN_POINT('Ctrl Pts',(21.8344580337528,-0.0698270680627233,
4.59401614113532));
#18328=CARTESIAN_POINT('Ctrl Pts',(21.8288454112575,1.47252919898561E-5,
4.59408074293421));
#18329=CARTESIAN_POINT('Ctrl Pts',(21.7211545887425,-1.54601956517634E-5,
4.59410286710644));
#18330=CARTESIAN_POINT('Ctrl Pts',(21.7229140916097,-0.0219078436841643,
4.59412557209431));
#18331=CARTESIAN_POINT('Ctrl Pts',(21.724673594477,-0.0437977792686499,
4.59293892497318));
#18332=CARTESIAN_POINT('Ctrl Pts',(21.7264330973443,-0.0655513867134097,
4.59052415646896));
#18333=CARTESIAN_POINT('Ctrl Pts',(21.7343857366881,-0.163873814968881,
4.57960983324176));
#18334=CARTESIAN_POINT('Ctrl Pts',(21.742338376032,-0.259411224460086,4.54360647774573));
#18335=CARTESIAN_POINT('Ctrl Pts',(21.7502910153758,-0.340482865683332,
4.48691599054611));
#18336=CARTESIAN_POINT('Ctrl Pts',(21.7582436547196,-0.421554506906578,
4.4302255033465));
#18337=CARTESIAN_POINT('Ctrl Pts',(21.7661962940634,-0.488160379861865,
4.3528478844433));
#18338=CARTESIAN_POINT('Ctrl Pts',(21.7741489334072,-0.532157009426634,
4.26424360160945));
#18339=CARTESIAN_POINT('Ctrl Pts',(21.782101572751,-0.576153638991403,4.1756393187756));
#18340=CARTESIAN_POINT('Ctrl Pts',(21.7900542120948,-0.597541025165654,
4.0758083720111));
#18341=CARTESIAN_POINT('Ctrl Pts',(21.7980068514386,-0.593704268699233,
3.9769564542281));
#18342=CARTESIAN_POINT('Ctrl Pts',(21.8059594907824,-0.589867512232813,
3.87810453644509));
#18343=CARTESIAN_POINT('Ctrl Pts',(21.8139121301262,-0.560806613125721,
3.78023164764359));
#18344=CARTESIAN_POINT('Ctrl Pts',(21.82186476947,-0.510074662095298,3.69530408148155));
#18345=CARTESIAN_POINT('Ctrl Pts',(21.8298174088138,-0.459342711064876,
3.61037651531951));
#18346=CARTESIAN_POINT('Ctrl Pts',(21.8377700481576,-0.386939708111122,
3.53839427179695));
#18347=CARTESIAN_POINT('Ctrl Pts',(21.8457226875014,-0.301717906454235,
3.48815816056295));
#18348=CARTESIAN_POINT('Ctrl Pts',(21.8536753268452,-0.216496104797349,
3.43792204932895));
#18349=CARTESIAN_POINT('Ctrl Pts',(21.8616279661891,-0.118455504437329,
3.40943207038352));
#18350=CARTESIAN_POINT('Ctrl Pts',(21.8695806055329,-0.0195829040543552,
3.40617151167847));
#18351=CARTESIAN_POINT('Ctrl Pts',(21.8775332448767,0.0792896963286298,
3.40291095297342));
#18352=CARTESIAN_POINT('Ctrl Pts',(21.8854858842205,0.178994296734569,3.42487981450875));
#18353=CARTESIAN_POINT('Ctrl Pts',(21.8934385235643,0.267340651814441,3.46939210375187));
#18354=CARTESIAN_POINT('Ctrl Pts',(21.9013911629081,0.355687006894294,3.51390439299499));
#18355=CARTESIAN_POINT('Ctrl Pts',(21.9093438022519,0.432675116648084,3.58096010994589));
#18356=CARTESIAN_POINT('Ctrl Pts',(21.9172964415957,0.488892136101412,3.66236077992681));
#18357=CARTESIAN_POINT('Ctrl Pts',(21.9252490809395,0.545109155554752,3.74376144990775));
#18358=CARTESIAN_POINT('Ctrl Pts',(21.9332017202833,0.580555084707621,3.8395070729187));
#18359=CARTESIAN_POINT('Ctrl Pts',(21.9411543596271,0.590896175957217,3.93789144251738));
#18360=CARTESIAN_POINT('Ctrl Pts',(21.9491069989709,0.601237267206812,4.03627581211605));
#18361=CARTESIAN_POINT('Ctrl Pts',(21.9570596383147,0.58647352055314,4.13729892830245));
#18362=CARTESIAN_POINT('Ctrl Pts',(21.9650122776585,0.548410005102802,4.22860933921557));
#18363=CARTESIAN_POINT('Ctrl Pts',(21.9729649170023,0.510346489652465,4.31991975012869));
#18364=CARTESIAN_POINT('Ctrl Pts',(21.9809175563462,0.448983205405461,4.40151745576853));
#18365=CARTESIAN_POINT('Ctrl Pts',(21.98887019569,0.371822649612145,4.46342602528218));
#18366=CARTESIAN_POINT('Ctrl Pts',(21.9968228350338,0.29466209381883,4.52533459479583));
#18367=CARTESIAN_POINT('Ctrl Pts',(22.0047754743776,0.201704266479203,4.5675540281833));
#18368=CARTESIAN_POINT('Ctrl Pts',(22.0127281137214,0.104314528045707,4.58492242469582));
#18369=CARTESIAN_POINT('Ctrl Pts',(22.0155369387284,0.069917050565085,4.59105683924014));
#18370=CARTESIAN_POINT('Ctrl Pts',(22.0183457637354,0.0349667096964542,
4.59409118517947));
#18371=CARTESIAN_POINT('Ctrl Pts',(22.0211545887425,1.20066176157995E-5,
4.59406577061205));
#18372=CARTESIAN_POINT('Origin',(4.,0.,4.));
#18373=CARTESIAN_POINT('',(22.4288454112575,5.18920962550018E-6,4.59405135764298));
#18374=CARTESIAN_POINT('',(22.3211545887424,-7.30827440488969E-6,4.59414400810326));
#18375=CARTESIAN_POINT('',(4.,-7.27562663373442E-17,4.5941));
#18376=CARTESIAN_POINT('Ctrl Pts',(22.4288454112575,5.18920962550018E-6,
4.59405135764298));
#18377=CARTESIAN_POINT('Ctrl Pts',(22.4253213780041,0.0438634191921666,
4.5940647188338));
#18378=CARTESIAN_POINT('Ctrl Pts',(22.4217973447507,0.0877187745911938,
4.589273164082));
#18379=CARTESIAN_POINT('Ctrl Pts',(22.4182733114973,0.130485535360993,4.57964583089408));
#18380=CARTESIAN_POINT('Ctrl Pts',(22.4103206721535,0.226996720088313,4.55791995512033));
#18381=CARTESIAN_POINT('Ctrl Pts',(22.4023680328097,0.317964089339764,4.51156722320365));
#18382=CARTESIAN_POINT('Ctrl Pts',(22.3944153934659,0.392265646131591,4.44625488916104));
#18383=CARTESIAN_POINT('Ctrl Pts',(22.3864627541221,0.4665672029234,4.38094255511845));
#18384=CARTESIAN_POINT('Ctrl Pts',(22.3785101147783,0.524202947255594,4.29667061894994));
#18385=CARTESIAN_POINT('Ctrl Pts',(22.3705574754345,0.558126122886914,4.20374247196213));
#18386=CARTESIAN_POINT('Ctrl Pts',(22.3626048360906,0.592049298518242,4.11081432497429));
#18387=CARTESIAN_POINT('Ctrl Pts',(22.3546521967468,0.602259905448686,4.00922996716717));
#18388=CARTESIAN_POINT('Ctrl Pts',(22.346699557403,0.587509558716917,3.91140947017845));
#18389=CARTESIAN_POINT('Ctrl Pts',(22.3387469180592,0.572759211985149,3.81358897318973));
#18390=CARTESIAN_POINT('Ctrl Pts',(22.3307942787154,0.533047911591167,3.71953233701942));
#18391=CARTESIAN_POINT('Ctrl Pts',(22.3228416393716,0.473230904440663,3.6407392662825));
#18392=CARTESIAN_POINT('Ctrl Pts',(22.3148890000278,0.413413897290173,3.5619461955456));
#18393=CARTESIAN_POINT('Ctrl Pts',(22.306936360684,0.333491183383171,3.49841669024209));
#18394=CARTESIAN_POINT('Ctrl Pts',(22.2989837213402,0.243234403245124,3.45791809774646));
#18395=CARTESIAN_POINT('Ctrl Pts',(22.2910310819964,0.152977623107077,3.41741950525082));
#18396=CARTESIAN_POINT('Ctrl Pts',(22.2830784426526,0.0523867767379842,
3.39995182556307));
#18397=CARTESIAN_POINT('Ctrl Pts',(22.2751258033088,-0.0462395349927855,
3.40765072037886));
#18398=CARTESIAN_POINT('Ctrl Pts',(22.267173163965,-0.144865846723578,3.41534961519466));
#18399=CARTESIAN_POINT('Ctrl Pts',(22.2592205246212,-0.241527623816046,
3.448215084514));
#18400=CARTESIAN_POINT('Ctrl Pts',(22.2512678852774,-0.324406647450603,
3.50222887712101));
#18401=CARTESIAN_POINT('Ctrl Pts',(22.2433152459336,-0.40728567108515,3.55624266972802));
#18402=CARTESIAN_POINT('Ctrl Pts',(22.2353626065897,-0.476381941261788,
3.63140478562268));
#18403=CARTESIAN_POINT('Ctrl Pts',(22.2274099672459,-0.523247497912515,
3.71852563243507));
#18404=CARTESIAN_POINT('Ctrl Pts',(22.2194573279021,-0.570113054563243,
3.80564647924745));
#18405=CARTESIAN_POINT('Ctrl Pts',(22.2115046885583,-0.59474789768806,3.90472605697756));
#18406=CARTESIAN_POINT('Ctrl Pts',(22.2035520492145,-0.594140082177443,
4.00365053781872));
#18407=CARTESIAN_POINT('Ctrl Pts',(22.1955994098707,-0.593532266666827,
4.10257501865988));
#18408=CARTESIAN_POINT('Ctrl Pts',(22.1876467705269,-0.567681792520777,
4.2013444026121));
#18409=CARTESIAN_POINT('Ctrl Pts',(22.1796941311831,-0.519749232289404,
4.2878827872712));
#18410=CARTESIAN_POINT('Ctrl Pts',(22.1717414918393,-0.471816672058032,
4.37442117193029));
#18411=CARTESIAN_POINT('Ctrl Pts',(22.1637888524955,-0.401802025741336,
4.44872855729627));
#18412=CARTESIAN_POINT('Ctrl Pts',(22.1558362131517,-0.318265537426909,
4.50171985346399));
#18413=CARTESIAN_POINT('Ctrl Pts',(22.1478835738079,-0.234729049112483,
4.55471114963171));
#18414=CARTESIAN_POINT('Ctrl Pts',(22.1399309344641,-0.137670718800326,
4.58638635660118));
#18415=CARTESIAN_POINT('Ctrl Pts',(22.1319782951203,-0.0389572492816432,
4.5928727489116));
#18416=CARTESIAN_POINT('Ctrl Pts',(22.1309340004994,-0.0259947671705595,
4.5937245044491));
#18417=CARTESIAN_POINT('Ctrl Pts',(22.1298897058784,-0.0130037447923657,
4.5941419185755));
#18418=CARTESIAN_POINT('Ctrl Pts',(22.1288454112575,-1.19684274697274E-5,
4.59413016891312));
#18419=CARTESIAN_POINT('Ctrl Pts',(22.0211545887425,1.20066176157995E-5,
4.59406577061205));
#18420=CARTESIAN_POINT('Ctrl Pts',(22.0262984030792,-0.064000704172389,
4.59401922879619));
#18421=CARTESIAN_POINT('Ctrl Pts',(22.031442217416,-0.128028044405449,4.5837112392356));
#18422=CARTESIAN_POINT('Ctrl Pts',(22.0365860317528,-0.188701337098646,
4.56338935830438));
#18423=CARTESIAN_POINT('Ctrl Pts',(22.0445386710966,-0.282505814282095,
4.53197053576284));
#18424=CARTESIAN_POINT('Ctrl Pts',(22.0524913104404,-0.368293119121642,
4.4766155310422));
#18425=CARTESIAN_POINT('Ctrl Pts',(22.0604439497842,-0.435574585201076,
4.40409224738955));
#18426=CARTESIAN_POINT('Ctrl Pts',(22.068396589128,-0.502856051280518,4.33156896373689));
#18427=CARTESIAN_POINT('Ctrl Pts',(22.0763492284718,-0.551631678599843,
4.24187740115222));
#18428=CARTESIAN_POINT('Ctrl Pts',(22.0843018678156,-0.575937982408454,
4.14598357473613));
#18429=CARTESIAN_POINT('Ctrl Pts',(22.0922545071594,-0.600244286217068,
4.05008974832002));
#18430=CARTESIAN_POINT('Ctrl Pts',(22.1002071465032,-0.600081266514962,
3.94799365807249));
#18431=CARTESIAN_POINT('Ctrl Pts',(22.1081597858471,-0.575468854681199,
3.85217794154701));
#18432=CARTESIAN_POINT('Ctrl Pts',(22.1161124251909,-0.550856442847438,
3.75636222502155));
#18433=CARTESIAN_POINT('Ctrl Pts',(22.1240650645347,-0.501794638882025,
3.66682688221814));
#18434=CARTESIAN_POINT('Ctrl Pts',(22.1320177038785,-0.434281916527717,
3.5945188282416));
#18435=CARTESIAN_POINT('Ctrl Pts',(22.1399703432223,-0.366769194173409,
3.52221077426505));
#18436=CARTESIAN_POINT('Ctrl Pts',(22.1479229825661,-0.280805553430205,
3.46713000911538));
#18437=CARTESIAN_POINT('Ctrl Pts',(22.1558756219099,-0.186901220180937,
3.43601090651668));
#18438=CARTESIAN_POINT('Ctrl Pts',(22.1638282612537,-0.0929968869316588,
3.40489180391798));
#18439=CARTESIAN_POINT('Ctrl Pts',(22.1717809005975,0.00884813882368474,
3.39773436387026));
#18440=CARTESIAN_POINT('Ctrl Pts',(22.1797335399413,0.106181915586414,3.41541368090248));
#18441=CARTESIAN_POINT('Ctrl Pts',(22.1876861792851,0.203515692349121,3.4330929979347));
#18442=CARTESIAN_POINT('Ctrl Pts',(22.1956388186289,0.296338220119215,3.47560907204686));
#18443=CARTESIAN_POINT('Ctrl Pts',(22.2035914579727,0.373300680656879,3.53776373412001));
#18444=CARTESIAN_POINT('Ctrl Pts',(22.2115440973165,0.450263141194552,3.59991839619317));
#18445=CARTESIAN_POINT('Ctrl Pts',(22.2194967366603,0.511365534499791,3.68171164622733));
#18446=CARTESIAN_POINT('Ctrl Pts',(22.2274493760041,0.549137260797828,3.7731431454068));
#18447=CARTESIAN_POINT('Ctrl Pts',(22.2354020153479,0.586908987095865,3.86457464458628));
#18448=CARTESIAN_POINT('Ctrl Pts',(22.2433546546918,0.6013500463867,3.96564439291107));
#18449=CARTESIAN_POINT('Ctrl Pts',(22.2513072940356,0.590694822479903,4.06399523710107));
#18450=CARTESIAN_POINT('Ctrl Pts',(22.2592599333794,0.580039598573106,4.16234608129106));
#18451=CARTESIAN_POINT('Ctrl Pts',(22.2672125727232,0.544288091468676,4.25797802134625));
#18452=CARTESIAN_POINT('Ctrl Pts',(22.275165212067,0.487811409852587,4.33919875012361));
#18453=CARTESIAN_POINT('Ctrl Pts',(22.2831178514108,0.431334728236497,4.42041947890096));
#18454=CARTESIAN_POINT('Ctrl Pts',(22.2910704907546,0.354132872108749,4.48722899640046));
#18455=CARTESIAN_POINT('Ctrl Pts',(22.2990231300984,0.265644819817582,4.53145892916239));
#18456=CARTESIAN_POINT('Ctrl Pts',(22.3064002829798,0.183560135512932,4.57248819778762));
#18457=CARTESIAN_POINT('Ctrl Pts',(22.3137774358611,0.0917635873240076,
4.59408754951618));
#18458=CARTESIAN_POINT('Ctrl Pts',(22.3211545887424,-7.30827440488969E-6,
4.59414400810326));
#18459=CARTESIAN_POINT('Origin',(4.,0.,4.));
#18460=CARTESIAN_POINT('',(22.7288454112575,-7.11440487624268E-7,4.59414971000239));
#18461=CARTESIAN_POINT('',(22.6211545887425,-1.51245797256638E-7,4.59404869726453));
#18462=CARTESIAN_POINT('',(4.,-7.27562663373442E-17,4.5941));
#18463=CARTESIAN_POINT('Ctrl Pts',(22.7288454112575,-7.11440487624268E-7,
4.59414971000239));
#18464=CARTESIAN_POINT('Ctrl Pts',(22.7287056894736,0.0017373052546791,
4.59414999869406));
#18465=CARTESIAN_POINT('Ctrl Pts',(22.7285659676897,0.0034753215591825,
4.59414251282321));
#18466=CARTESIAN_POINT('Ctrl Pts',(22.7284262459057,0.00521327185949689,
4.59412723628209));
#18467=CARTESIAN_POINT('Ctrl Pts',(22.7204736065619,0.104133365400505,4.59325773105135));
#18468=CARTESIAN_POINT('Ctrl Pts',(22.7125209672181,0.202839630323109,4.56714939948764));
#18469=CARTESIAN_POINT('Ctrl Pts',(22.7045683278743,0.289252680684759,4.51898953373575));
#18470=CARTESIAN_POINT('Ctrl Pts',(22.6966156885305,0.375665731046408,4.47082966798385));
#18471=CARTESIAN_POINT('Ctrl Pts',(22.6886630491867,0.449785566847107,4.40061826804377));
#18472=CARTESIAN_POINT('Ctrl Pts',(22.6807104098429,0.502555912967013,4.31694216252228));
#18473=CARTESIAN_POINT('Ctrl Pts',(22.6727577704991,0.555326259086918,4.23326605700079));
#18474=CARTESIAN_POINT('Ctrl Pts',(22.6648051311553,0.586747115526033,4.13612524589788));
#18475=CARTESIAN_POINT('Ctrl Pts',(22.6568524918115,0.592973744123511,4.03739517928057));
#18476=CARTESIAN_POINT('Ctrl Pts',(22.6488998524677,0.59920037272099,3.93866511266326));
#18477=CARTESIAN_POINT('Ctrl Pts',(22.6409472131239,0.580232773476834,3.83834579053153));
#18478=CARTESIAN_POINT('Ctrl Pts',(22.6329945737801,0.538391640361539,3.74870332422701));
#18479=CARTESIAN_POINT('Ctrl Pts',(22.6250419344363,0.496550507246239,3.65906085792248));
#18480=CARTESIAN_POINT('Ctrl Pts',(22.6170892950925,0.431835840259791,3.58009524744515));
#18481=CARTESIAN_POINT('Ctrl Pts',(22.6091366557487,0.35215901686313,3.52146073929621));
#18482=CARTESIAN_POINT('Ctrl Pts',(22.6011840164048,0.272482193466486,3.46282623114728));
#18483=CARTESIAN_POINT('Ctrl Pts',(22.593231377061,0.17784321365963,3.42452282532672));
#18484=CARTESIAN_POINT('Ctrl Pts',(22.5852787377172,0.0798134434713266,
3.41123383340666));
#18485=CARTESIAN_POINT('Ctrl Pts',(22.5773260983734,-0.0182163267169884,
3.3979448414866));
#18486=CARTESIAN_POINT('Ctrl Pts',(22.5693734590296,-0.119636887286728,
3.40967026346704));
#18487=CARTESIAN_POINT('Ctrl Pts',(22.5614208196858,-0.212048437952692,
3.44497640167274));
#18488=CARTESIAN_POINT('Ctrl Pts',(22.553468180342,-0.304459988618666,3.48028253987845));
#18489=CARTESIAN_POINT('Ctrl Pts',(22.5455155409982,-0.387862529380837,
3.53916939430943));
#18490=CARTESIAN_POINT('Ctrl Pts',(22.5375629016544,-0.452058834188948,
3.61443730067171));
#18491=CARTESIAN_POINT('Ctrl Pts',(22.5296102623106,-0.516255138997059,
3.689705207034));
#18492=CARTESIAN_POINT('Ctrl Pts',(22.5216576229668,-0.561245207851117,
3.7813541653276));
#18493=CARTESIAN_POINT('Ctrl Pts',(22.513704983623,-0.581528460676763,3.87817881267738));
#18494=CARTESIAN_POINT('Ctrl Pts',(22.5057523442792,-0.601811713502406,
3.97500346002715));
#18495=CARTESIAN_POINT('Ctrl Pts',(22.4977997049354,-0.597388150299644,
4.07700379643311));
#18496=CARTESIAN_POINT('Ctrl Pts',(22.4898470655916,-0.568798575589296,
4.17170890717095));
#18497=CARTESIAN_POINT('Ctrl Pts',(22.4818944262477,-0.540209000878948,
4.26641401790879));
#18498=CARTESIAN_POINT('Ctrl Pts',(22.4739417869039,-0.487453414661012,
4.35382390297851));
#18499=CARTESIAN_POINT('Ctrl Pts',(22.4659891475601,-0.416981925106977,
4.42325150516024));
#18500=CARTESIAN_POINT('Ctrl Pts',(22.4580365082163,-0.346510435552941,
4.49267910734197));
#18501=CARTESIAN_POINT('Ctrl Pts',(22.4500838688725,-0.258323042662803,
4.54412442663572));
#18502=CARTESIAN_POINT('Ctrl Pts',(22.4421312295287,-0.163201846116148,
4.57129757646718));
#18503=CARTESIAN_POINT('Ctrl Pts',(22.4377026234383,-0.11023146834083,4.58642955613285));
#18504=CARTESIAN_POINT('Ctrl Pts',(22.4332740173479,-0.0551108697057404,
4.59403456681078));
#18505=CARTESIAN_POINT('Ctrl Pts',(22.4288454112575,5.18920962550018E-6,
4.59405135764298));
#18506=CARTESIAN_POINT('Ctrl Pts',(22.3211545887424,-7.30827440488969E-6,
4.59414400810326));
#18507=CARTESIAN_POINT('Ctrl Pts',(22.3217300752049,-0.00716629073194701,
4.59414841239758));
#18508=CARTESIAN_POINT('Ctrl Pts',(22.3223055616673,-0.0143251170819474,
4.59402171850555));
#18509=CARTESIAN_POINT('Ctrl Pts',(22.3228810481298,-0.0214791647150919,
4.59376292335171));
#18510=CARTESIAN_POINT('Ctrl Pts',(22.3308336874736,-0.120340848501978,
4.59018663675477));
#18511=CARTESIAN_POINT('Ctrl Pts',(22.3387863268174,-0.218289967621164,
4.56138371553656));
#18512=CARTESIAN_POINT('Ctrl Pts',(22.3467389661612,-0.303350908332583,
4.51087570903952));
#18513=CARTESIAN_POINT('Ctrl Pts',(22.3546916055051,-0.388411849044011,
4.46036770254246));
#18514=CARTESIAN_POINT('Ctrl Pts',(22.3626442448489,-0.460584611347669,
4.38815461076656));
#18515=CARTESIAN_POINT('Ctrl Pts',(22.3705968841927,-0.511045091866278,
4.3030654678256));
#18516=CARTESIAN_POINT('Ctrl Pts',(22.3785495235365,-0.561505572384874,
4.21797632488466));
#18517=CARTESIAN_POINT('Ctrl Pts',(22.3865021628803,-0.590253771118432,
4.12001113077866));
#18518=CARTESIAN_POINT('Ctrl Pts',(22.3944548022241,-0.593774829630164,
4.02114746451658));
#18519=CARTESIAN_POINT('Ctrl Pts',(22.4024074415679,-0.597295888141896,
3.92228379825449));
#18520=CARTESIAN_POINT('Ctrl Pts',(22.4103600809117,-0.575589806431797,
3.82252165983632));
#18521=CARTESIAN_POINT('Ctrl Pts',(22.4183127202555,-0.531310447862662,
3.73405832985033));
#18522=CARTESIAN_POINT('Ctrl Pts',(22.4262653595993,-0.487031089293526,
3.64559499986435));
#18523=CARTESIAN_POINT('Ctrl Pts',(22.4342179989431,-0.420178453865353,
3.56843047831055));
#18524=CARTESIAN_POINT('Ctrl Pts',(22.4421706382869,-0.338926188203527,
3.51199917808983));
#18525=CARTESIAN_POINT('Ctrl Pts',(22.4501232776307,-0.257673922541701,
3.45556787786912));
#18526=CARTESIAN_POINT('Ctrl Pts',(22.4580759169745,-0.162022026646223,
3.41986979898149));
#18527=CARTESIAN_POINT('Ctrl Pts',(22.4660285563183,-0.0636652448434586,
3.40926951931498));
#18528=CARTESIAN_POINT('Ctrl Pts',(22.4739811956621,0.0346915369593057,
3.39866923964846));
#18529=CARTESIAN_POINT('Ctrl Pts',(22.4819338350059,0.135753204669356,3.41316675920307));
#18530=CARTESIAN_POINT('Ctrl Pts',(22.4898864743497,0.227163587879617,3.45098955584192));
#18531=CARTESIAN_POINT('Ctrl Pts',(22.4978391136936,0.318573971089878,3.48881235248077));
#18532=CARTESIAN_POINT('Ctrl Pts',(22.5057917530374,0.40033306980035,3.54996042620388));
#18533=CARTESIAN_POINT('Ctrl Pts',(22.5137443923812,0.462444730281743,3.62695759769032));
#18534=CARTESIAN_POINT('Ctrl Pts',(22.521697031725,0.524556390763143,3.70395476917678));
#18535=CARTESIAN_POINT('Ctrl Pts',(22.5296496710688,0.567020613015458,3.79680103842659));
#18536=CARTESIAN_POINT('Ctrl Pts',(22.5376023104126,0.584645549343987,3.89414467407578));
#18537=CARTESIAN_POINT('Ctrl Pts',(22.5455549497564,0.602270485672515,3.99148830972497));
#18538=CARTESIAN_POINT('Ctrl Pts',(22.5535075891002,0.595056136077256,4.09332931177355));
#18539=CARTESIAN_POINT('Ctrl Pts',(22.561460228444,0.563884587368514,4.18721625032571));
#18540=CARTESIAN_POINT('Ctrl Pts',(22.5694128677878,0.532713038659782,4.28110318887784));
#18541=CARTESIAN_POINT('Ctrl Pts',(22.5773655071316,0.477584290837583,4.36703606393356));
#18542=CARTESIAN_POINT('Ctrl Pts',(22.5853181464754,0.405238519368296,4.43450837402952));
#18543=CARTESIAN_POINT('Ctrl Pts',(22.5932707858192,0.332892747898984,4.5019806841255));
#18544=CARTESIAN_POINT('Ctrl Pts',(22.601223425163,0.24332995278257,4.55099242926169));
#18545=CARTESIAN_POINT('Ctrl Pts',(22.6091760645068,0.14750052788588,4.57555132613148));
#18546=CARTESIAN_POINT('Ctrl Pts',(22.6131689059187,0.0993867282199646,
4.58788179608141));
#18547=CARTESIAN_POINT('Ctrl Pts',(22.6171617473306,0.0496932250345643,
4.5940481472271));
#18548=CARTESIAN_POINT('Ctrl Pts',(22.6211545887425,-1.51173456864708E-7,
4.59404872180247));
#18549=CARTESIAN_POINT('Origin',(3.42660065607856,0.,4.));
#18550=CARTESIAN_POINT('',(22.7766006560786,-4.98014040841517E-7,4.41590979742004));
#18551=CARTESIAN_POINT('',(22.8,4.87367679877478E-13,4.415875));
#18552=CARTESIAN_POINT('',(3.42660065607856,4.87367679877478E-13,4.415875));
#18553=CARTESIAN_POINT('',(22.8,-0.195748955928421,4.36692555359082));
#18554=CARTESIAN_POINT('Ctrl Pts',(22.7766006560786,-4.98014040834069E-7,
4.41590979742004));
#18555=CARTESIAN_POINT('Ctrl Pts',(22.7844004373857,-0.0679170312443507,
4.41589851620688));
#18556=CARTESIAN_POINT('Ctrl Pts',(22.7922002186928,-0.135834416676695,
4.39892762624317));
#18557=CARTESIAN_POINT('Ctrl Pts',(22.8,-0.195762566582618,4.36695865185838));
#18558=CARTESIAN_POINT('Origin',(22.8,0.,4.));
#18559=CARTESIAN_POINT('Origin',(3.42660065607856,0.,4.));
#18560=CARTESIAN_POINT('',(22.4766006560785,3.63249072247605E-6,4.41584094994071));
#18561=CARTESIAN_POINT('',(22.5733993439214,-1.05822049303872E-7,4.41583910483016));
#18562=CARTESIAN_POINT('',(3.42660065607856,4.87367679877478E-13,4.415875));
#18563=CARTESIAN_POINT('Ctrl Pts',(22.4766006560785,3.63249072248342E-6,
4.41584094994071));
#18564=CARTESIAN_POINT('Ctrl Pts',(22.4810292621689,-0.0385780726118879,
4.41582919621688));
#18565=CARTESIAN_POINT('Ctrl Pts',(22.4934105076031,-0.146451497349971,
4.40094585736882));
#18566=CARTESIAN_POINT('Ctrl Pts',(22.5137443923812,-0.304292138366774,
4.30886736509782));
#18567=CARTESIAN_POINT('Ctrl Pts',(22.5376023104126,-0.415080201412036,
4.12530439950267));
#18568=CARTESIAN_POINT('Ctrl Pts',(22.561460228444,-0.424369795825249,3.91110111771763));
#18569=CARTESIAN_POINT('Ctrl Pts',(22.5853181464754,-0.329889515310188,
3.71863599132299));
#18570=CARTESIAN_POINT('Ctrl Pts',(22.6091760645068,-0.154742073939436,
3.59497211022641));
#18571=CARTESIAN_POINT('Ctrl Pts',(22.6330339825383,0.0582436639512456,
3.57034842802071));
#18572=CARTESIAN_POINT('Ctrl Pts',(22.6568919005697,0.256987911016647,3.65078654733876));
#18573=CARTESIAN_POINT('Ctrl Pts',(22.6807498186011,0.39289034562191,3.81661632308649));
#18574=CARTESIAN_POINT('Ctrl Pts',(22.7046077366325,0.432722782933869,4.02728943245291));
#18575=CARTESIAN_POINT('Ctrl Pts',(22.7284656546639,0.366738191089385,4.2312875884069));
#18576=CARTESIAN_POINT('Ctrl Pts',(22.7523235726953,0.211084664509997,4.37873330099785));
#18577=CARTESIAN_POINT('Ctrl Pts',(22.7683685731669,0.0716802821347026,
4.41560650088387));
#18578=CARTESIAN_POINT('Ctrl Pts',(22.7764609342946,0.00121612829983627,
4.41590999950663));
#18579=CARTESIAN_POINT('Ctrl Pts',(22.7766006560786,-4.98014040834069E-7,
4.41590979742004));
#18580=CARTESIAN_POINT('',(22.8,0.415641328671541,4.01393920819689));
#18581=CARTESIAN_POINT('Origin',(22.8,0.,4.));
#18582=CARTESIAN_POINT('Ctrl Pts',(22.5733993439214,-1.0582204931428E-7,
4.41583910483016));
#18583=CARTESIAN_POINT('Ctrl Pts',(22.5773591418533,-0.034498011376554,
4.41583950370926));
#18584=CARTESIAN_POINT('Ctrl Pts',(22.5892715791291,-0.138279341065089,
4.40307041914735));
#18585=CARTESIAN_POINT('Ctrl Pts',(22.6091366557487,-0.295063722636797,
4.31769517074077));
#18586=CARTESIAN_POINT('Ctrl Pts',(22.6329945737801,-0.411209141905604,
4.13747522778479));
#18587=CARTESIAN_POINT('Ctrl Pts',(22.6568524918115,-0.426804986482714,
3.92363755172126));
#18588=CARTESIAN_POINT('Ctrl Pts',(22.6807104098429,-0.33803111495158,3.72847502015617));
#18589=CARTESIAN_POINT('Ctrl Pts',(22.7045683278743,-0.16660749730952,3.59970312177549));
#18590=CARTESIAN_POINT('Ctrl Pts',(22.7284262459057,0.0455714674079685,
3.56882345794434));
#18591=CARTESIAN_POINT('Ctrl Pts',(22.7522841639372,0.246577802732478,3.64336153500176));
#18592=CARTESIAN_POINT('Ctrl Pts',(22.7761420819686,0.387346815298129,3.80514019809748));
#18593=CARTESIAN_POINT('Ctrl Pts',(22.7920473606562,0.417963038852713,3.94471011778788));
#18594=CARTESIAN_POINT('Ctrl Pts',(22.8,0.415641328671541,4.01393920819689));
#18595=CARTESIAN_POINT('Origin',(3.42660065607856,0.,4.));
#18596=CARTESIAN_POINT('',(22.1766006560786,-8.37799962078257E-6,4.41589611849309));
#18597=CARTESIAN_POINT('',(22.2733993439214,-5.11585294796223E-6,4.41590580604266));
#18598=CARTESIAN_POINT('',(3.42660065607856,4.87367679877478E-13,4.415875));
#18599=CARTESIAN_POINT('Ctrl Pts',(22.1766006560786,-8.37799962077716E-6,
4.41589611849309));
#18600=CARTESIAN_POINT('Ctrl Pts',(22.1776449506995,-0.0091027307950905,
4.41590434335565));
#18601=CARTESIAN_POINT('Ctrl Pts',(22.1866418846642,-0.0874489573854402,
4.4133870032437));
#18602=CARTESIAN_POINT('Ctrl Pts',(22.2035914579727,-0.232253957950086,
4.36612956178204));
#18603=CARTESIAN_POINT('Ctrl Pts',(22.2274493760041,-0.379286482964224,
4.21008217638027));
#18604=CARTESIAN_POINT('Ctrl Pts',(22.2513072940356,-0.433573131350875,
4.00266397632408));
#18605=CARTESIAN_POINT('Ctrl Pts',(22.275165212067,-0.381839338801546,3.79459436150246));
#18606=CARTESIAN_POINT('Ctrl Pts',(22.2990231300984,-0.236735426869051,
3.63675202040985));
#18607=CARTESIAN_POINT('Ctrl Pts',(22.3228810481298,-0.0337432544318164,
3.56773370504276));
#18608=CARTESIAN_POINT('Ctrl Pts',(22.3467389661613,0.177500062688638,3.60441627341574));
#18609=CARTESIAN_POINT('Ctrl Pts',(22.3705968841926,0.345339779804043,3.73782983856348));
#18610=CARTESIAN_POINT('Ctrl Pts',(22.3944548022241,0.428734513273282,3.93535114928888));
#18611=CARTESIAN_POINT('Ctrl Pts',(22.4183127202555,0.407291980919218,4.1486808655136));
#18612=CARTESIAN_POINT('Ctrl Pts',(22.4421706382869,0.286255462618544,4.32565405918856));
#18613=CARTESIAN_POINT('Ctrl Pts',(22.4615999502279,0.130682174689606,4.40492695636159));
#18614=CARTESIAN_POINT('Ctrl Pts',(22.4730766228251,0.0307047625933256,
4.41585030288671));
#18615=CARTESIAN_POINT('Ctrl Pts',(22.4766006560785,3.63249072248342E-6,
4.41584094994071));
#18616=CARTESIAN_POINT('Ctrl Pts',(22.2733993439214,-5.11585294797612E-6,
4.41590580604266));
#18617=CARTESIAN_POINT('Ctrl Pts',(22.2739748303838,-0.0050164638240448,
4.41590888908576));
#18618=CARTESIAN_POINT('Ctrl Pts',(22.2825029561901,-0.0792779396689182,
4.41459464077989));
#18619=CARTESIAN_POINT('Ctrl Pts',(22.2989837213402,-0.221370022215225,
4.37281103827166));
#18620=CARTESIAN_POINT('Ctrl Pts',(22.3228416393716,-0.372934645290675,
4.22116172228637));
#18621=CARTESIAN_POINT('Ctrl Pts',(22.346699557403,-0.43330658847365,4.01543234121164));
#18622=CARTESIAN_POINT('Ctrl Pts',(22.3705574754345,-0.387723268841402,
3.80592933171158));
#18623=CARTESIAN_POINT('Ctrl Pts',(22.3944153934659,-0.247331046528593,
3.64388188817752));
#18624=CARTESIAN_POINT('Ctrl Pts',(22.4182733114973,-0.0464596501027702,
3.56891502119853));
#18625=CARTESIAN_POINT('Ctrl Pts',(22.4421312295287,0.165772403721094,3.59936017830047));
#18626=CARTESIAN_POINT('Ctrl Pts',(22.4659891475602,0.337468575289321,3.7277726770023));
#18627=CARTESIAN_POINT('Ctrl Pts',(22.4898470655915,0.426644514167594,3.92275218663495));
#18628=CARTESIAN_POINT('Ctrl Pts',(22.513704983623,0.411494197867752,4.13662086224655));
#18629=CARTESIAN_POINT('Ctrl Pts',(22.5375629016544,0.295722435535401,4.31708206952049));
#18630=CARTESIAN_POINT('Ctrl Pts',(22.5574610217539,0.138855410360913,4.40292493148274));
#18631=CARTESIAN_POINT('Ctrl Pts',(22.5694065025095,0.0347856757474044,
4.41583870262252));
#18632=CARTESIAN_POINT('Ctrl Pts',(22.5733993439214,-1.0582204931428E-7,
4.41583910483016));
#18633=CARTESIAN_POINT('Origin',(3.42660065607856,0.,4.));
#18634=CARTESIAN_POINT('',(21.8766006560786,1.03078286340212E-5,4.41586151989188));
#18635=CARTESIAN_POINT('',(21.9733993439214,8.40473402259622E-6,4.41585103914036));
#18636=CARTESIAN_POINT('',(3.42660065607856,4.87367679877478E-13,4.415875));
#18637=CARTESIAN_POINT('Ctrl Pts',(21.8766006560786,1.03078286340201E-5,
4.41586151989188));
#18638=CARTESIAN_POINT('Ctrl Pts',(21.8822132785738,-0.0488795353146484,
4.415816298089));
#18639=CARTESIAN_POINT('Ctrl Pts',(21.8957785404128,-0.167079919178725,
4.39498170153279));
#18640=CARTESIAN_POINT('Ctrl Pts',(21.9172964415957,-0.326407159500644,
4.28539643168872));
#18641=CARTESIAN_POINT('Ctrl Pts',(21.9411543596271,-0.423245389017799,
4.09410684177624));
#18642=CARTESIAN_POINT('Ctrl Pts',(21.9650122776585,-0.416588591947193,
3.87980556563057));
#18643=CARTESIAN_POINT('Ctrl Pts',(21.98887019569,-0.30806453650007,3.69489510271888));
#18644=CARTESIAN_POINT('Ctrl Pts',(22.0127281137213,-0.12421031036921,3.58459109808296));
#18645=CARTESIAN_POINT('Ctrl Pts',(22.0365860317528,0.0900167200678817,
3.57586588547707));
#18646=CARTESIAN_POINT('Ctrl Pts',(22.0604439497842,0.282232210442068,3.67085301705332));
#18647=CARTESIAN_POINT('Ctrl Pts',(22.0843018678157,0.405434237512275,3.8463255517439));
#18648=CARTESIAN_POINT('Ctrl Pts',(22.108159785847,0.429496549703537,4.05937567504088));
#18649=CARTESIAN_POINT('Ctrl Pts',(22.1320177038785,0.348535256241736,4.25790682842971));
#18650=CARTESIAN_POINT('Ctrl Pts',(22.1548313272889,0.18962186617866,4.38744320371645));
#18651=CARTESIAN_POINT('Ctrl Pts',(22.1696923113557,0.0601536901409818,
4.41584170838249));
#18652=CARTESIAN_POINT('Ctrl Pts',(22.1766006560786,-8.37799962077716E-6,
4.41589611849309));
#18653=CARTESIAN_POINT('Ctrl Pts',(21.9733993439214,8.40473402260317E-6,
4.41585103914036));
#18654=CARTESIAN_POINT('Ctrl Pts',(21.9785431582582,-0.044801031555974,
4.41581845947763));
#18655=CARTESIAN_POINT('Ctrl Pts',(21.9916396119388,-0.158914563981884,
4.39744691543598));
#18656=CARTESIAN_POINT('Ctrl Pts',(22.0126887049632,-0.317860118355158,
4.29488591379237));
#18657=CARTESIAN_POINT('Ctrl Pts',(22.0365466229946,-0.420290167226249,
4.10653136780738));
#18658=CARTESIAN_POINT('Ctrl Pts',(22.060404541026,-0.419947821735935,3.89212700053744));
#18659=CARTESIAN_POINT('Ctrl Pts',(22.0842624590574,-0.316916794682727,
3.70410052003731));
#18660=CARTESIAN_POINT('Ctrl Pts',(22.1081203770888,-0.136390978688423,
3.58842952252864));
#18661=CARTESIAN_POINT('Ctrl Pts',(22.1319782951203,0.0774861468089536,
3.57339871771534));
#18662=CARTESIAN_POINT('Ctrl Pts',(22.1558362131517,0.27241579873489,3.66268354680831));
#18663=CARTESIAN_POINT('Ctrl Pts',(22.1796941311831,0.400732367405962,3.83445143701846));
#18664=CARTESIAN_POINT('Ctrl Pts',(22.2035520492145,0.431058956528623,4.04670046033727));
#18665=CARTESIAN_POINT('Ctrl Pts',(22.227409967246,0.355979888945518,4.24752994899471));
#18666=CARTESIAN_POINT('Ctrl Pts',(22.2506923988149,0.197764744804664,4.38444734931837));
#18667=CARTESIAN_POINT('Ctrl Pts',(22.26602219104,0.064235283418036,4.41586628455644));
#18668=CARTESIAN_POINT('Ctrl Pts',(22.2733993439214,-5.11585294797612E-6,
4.41590580604266));
#18669=CARTESIAN_POINT('Origin',(3.42660065607856,0.,4.));
#18670=CARTESIAN_POINT('',(21.5766006560785,-1.05752387382048E-5,4.41586434469346));
#18671=CARTESIAN_POINT('',(21.6733993439214,-1.08222664516599E-5,4.41587700699864));
#18672=CARTESIAN_POINT('',(3.42660065607856,4.87367679877478E-13,4.415875));
#18673=CARTESIAN_POINT('Ctrl Pts',(21.5766006560785,-1.05752387381843E-5,
4.41586434469346));
#18674=CARTESIAN_POINT('Ctrl Pts',(21.5788289671043,-0.0194203346498642,
4.41588296395747));
#18675=CARTESIAN_POINT('Ctrl Pts',(21.5890099174739,-0.10809016089515,4.40978779866957));
#18676=CARTESIAN_POINT('Ctrl Pts',(21.6071435071872,-0.258824259222961,
4.34785450957493));
#18677=CARTESIAN_POINT('Ctrl Pts',(21.6310014252187,-0.39385182381868,4.18131050126406));
#18678=CARTESIAN_POINT('Ctrl Pts',(21.6548593432501,-0.432571889182456,
3.97043113659525));
#18679=CARTESIAN_POINT('Ctrl Pts',(21.6787172612815,-0.365516344619441,
3.76678216446856));
#18680=CARTESIAN_POINT('Ctrl Pts',(21.702575179313,-0.209082097331647,3.62016130585559));
#18681=CARTESIAN_POINT('Ctrl Pts',(21.7264330973443,-0.00152158196427748,
3.56642135455923));
#18682=CARTESIAN_POINT('Ctrl Pts',(21.7502910153758,0.206411001640417,3.61870319251831));
#18683=CARTESIAN_POINT('Ctrl Pts',(21.7741489334072,0.363870472821225,3.76422248622317));
#18684=CARTESIAN_POINT('Ctrl Pts',(21.7980068514386,0.432353701764573,3.96739580449697));
#18685=CARTESIAN_POINT('Ctrl Pts',(21.82186476947,0.395114673548107,4.17854173669174));
#18686=CARTESIAN_POINT('Ctrl Pts',(21.8457226875014,0.261259344941517,4.3460293508861));
#18687=CARTESIAN_POINT('Ctrl Pts',(21.8639679830376,0.110037800305057,4.4094070875278));
#18688=CARTESIAN_POINT('Ctrl Pts',(21.87426063923,0.0203934810735595,4.41588037378429));
#18689=CARTESIAN_POINT('Ctrl Pts',(21.8766006560786,1.03078286340201E-5,
4.41586151989188));
#18690=CARTESIAN_POINT('Ctrl Pts',(21.6733993439214,-1.0822266451653E-5,
4.41587700699864));
#18691=CARTESIAN_POINT('Ctrl Pts',(21.6751588467887,-0.0153356749568721,
4.41589290068126));
#18692=CARTESIAN_POINT('Ctrl Pts',(21.6848709889998,-0.0999166717736498,
4.41130778913604));
#18693=CARTESIAN_POINT('Ctrl Pts',(21.7025357705547,-0.248467031045983,
4.35532645760922));
#18694=CARTESIAN_POINT('Ctrl Pts',(21.7263936885861,-0.388341045935521,
4.1928315042612));
#18695=CARTESIAN_POINT('Ctrl Pts',(21.7502516066176,-0.433255096896122,
3.98318399549658));
#18696=CARTESIAN_POINT('Ctrl Pts',(21.774109524649,-0.372226475033738,3.77764845789182));
#18697=CARTESIAN_POINT('Ctrl Pts',(21.7979674426804,-0.220178340780001,
3.62648392906691));
#18698=CARTESIAN_POINT('Ctrl Pts',(21.8218253607118,-0.0142906046679706,
3.56665425395863));
#18699=CARTESIAN_POINT('Ctrl Pts',(21.8456832787432,0.195091573553633,3.61278941785858));
#18700=CARTESIAN_POINT('Ctrl Pts',(21.8695411967747,0.356768547853618,3.75360811649661));
#18701=CARTESIAN_POINT('Ctrl Pts',(21.8933991148061,0.431205894023261,3.95467634223136));
#18702=CARTESIAN_POINT('Ctrl Pts',(21.9172570328375,0.400201653291494,4.16682743688221));
#18703=CARTESIAN_POINT('Ctrl Pts',(21.941114950869,0.271337207055788,4.33818467892719));
#18704=CARTESIAN_POINT('Ctrl Pts',(21.9598290545635,0.118211900824938,4.40773087908456));
#18705=CARTESIAN_POINT('Ctrl Pts',(21.9705905189143,0.0244769910710258,
4.41586882955141));
#18706=CARTESIAN_POINT('Ctrl Pts',(21.9733993439214,8.40473402260317E-6,
4.41585103914036));
#18707=CARTESIAN_POINT('Origin',(3.42660065607856,0.,4.));
#18708=CARTESIAN_POINT('',(21.2766006560785,8.9771325895615E-6,4.41589335210553));
#18709=CARTESIAN_POINT('',(21.3733993439214,1.06214664634743E-5,4.41588075133303));
#18710=CARTESIAN_POINT('',(3.42660065607856,4.87367679877478E-13,4.415875));
#18711=CARTESIAN_POINT('Ctrl Pts',(21.2766006560785,8.97713258955941E-6,
4.41589335210553));
#18712=CARTESIAN_POINT('Ctrl Pts',(21.2833972949786,-0.0591814269577189,
4.41583723296416));
#18713=CARTESIAN_POINT('Ctrl Pts',(21.2981465732225,-0.187680420990878,
4.38813575385326));
#18714=CARTESIAN_POINT('Ctrl Pts',(21.3208484908102,-0.346716519889314,
4.26034671465164));
#18715=CARTESIAN_POINT('Ctrl Pts',(21.3447064088417,-0.429069235164158,
4.0623886883135));
#18716=CARTESIAN_POINT('Ctrl Pts',(21.368564326873,-0.406502834830527,3.8491749282489));
#18717=CARTESIAN_POINT('Ctrl Pts',(21.3924222449045,-0.284535418465691,
3.67284200661995));
#18718=CARTESIAN_POINT('Ctrl Pts',(21.4162801629359,-0.0929913416969399,
3.5765081259772));
#18719=CARTESIAN_POINT('Ctrl Pts',(21.4401380809674,0.121291651150069,3.58372954422009));
#18720=CARTESIAN_POINT('Ctrl Pts',(21.4639959989987,0.305915531372611,3.69274042788069));
#18721=CARTESIAN_POINT('Ctrl Pts',(21.4878539170302,0.415734731202803,3.87688464650718));
#18722=CARTESIAN_POINT('Ctrl Pts',(21.5117118350615,0.423895464867194,4.09113392265755));
#18723=CARTESIAN_POINT('Ctrl Pts',(21.535569753093,0.328402210690932,4.28309847227994));
#18724=CARTESIAN_POINT('Ctrl Pts',(21.5571993600986,0.169024930905334,4.39437398220882));
#18725=CARTESIAN_POINT('Ctrl Pts',(21.5708763277605,0.0498513310028489,
4.41581651349798));
#18726=CARTESIAN_POINT('Ctrl Pts',(21.5766006560785,-1.05752387381843E-5,
4.41586434469346));
#18727=CARTESIAN_POINT('Ctrl Pts',(21.3733993439214,1.06214664634605E-5,
4.41588075133303));
#18728=CARTESIAN_POINT('Ctrl Pts',(21.379727174663,-0.0551018547626871,
4.41582358345633));
#18729=CARTESIAN_POINT('Ctrl Pts',(21.3940076447484,-0.1795281855266,4.39095386216025));
#18730=CARTESIAN_POINT('Ctrl Pts',(21.4162407541777,-0.338898428465248,
4.27044521104599));
#18731=CARTESIAN_POINT('Ctrl Pts',(21.4400986722091,-0.427045644525908,
4.07499849655415));
#18732=CARTESIAN_POINT('Ctrl Pts',(21.4639565902406,-0.410768568010174,
3.86121260673678));
#18733=CARTESIAN_POINT('Ctrl Pts',(21.4878145082719,-0.294047387504818,
3.68136401506497));
#18734=CARTESIAN_POINT('Ctrl Pts',(21.5116724263034,-0.105423611064507,
3.57943060117972));
#18735=CARTESIAN_POINT('Ctrl Pts',(21.5355303443348,0.108979109962582,3.58033786138646));
#18736=CARTESIAN_POINT('Ctrl Pts',(21.5593882623662,0.296733470072461,3.68386394585134));
#18737=CARTESIAN_POINT('Ctrl Pts',(21.5832461803976,0.411928413892185,3.86469390692879));
#18738=CARTESIAN_POINT('Ctrl Pts',(21.6071040984291,0.426395639810567,4.07860989342611));
#18739=CARTESIAN_POINT('Ctrl Pts',(21.6309620164605,0.33659751701124,4.27330361969026));
#18740=CARTESIAN_POINT('Ctrl Pts',(21.6530604316246,0.177184770587036,4.39173732935402));
#18741=CARTESIAN_POINT('Ctrl Pts',(21.6672062074449,0.0539299276789421,
4.41582106406873));
#18742=CARTESIAN_POINT('Ctrl Pts',(21.6733993439214,-1.0822266451653E-5,
4.41587700699864));
#18743=CARTESIAN_POINT('Origin',(3.42660065607856,0.,4.));
#18744=CARTESIAN_POINT('',(20.9766006560786,-4.48287659654576E-6,4.41584197426197));
#18745=CARTESIAN_POINT('',(21.0733993439214,-7.65157297119567E-6,4.41584853425778));
#18746=CARTESIAN_POINT('',(3.42660065607856,4.87367679877478E-13,4.415875));
#18747=CARTESIAN_POINT('Ctrl Pts',(20.9766006560786,-4.48287659652116E-6,
4.41584197426197));
#18748=CARTESIAN_POINT('Ctrl Pts',(20.9800129835092,-0.0297322302090305,
4.41585318364051));
#18749=CARTESIAN_POINT('Ctrl Pts',(20.9913779502836,-0.128734546054536,
4.40538471300776));
#18750=CARTESIAN_POINT('Ctrl Pts',(21.0106955564018,-0.28396276796243,4.32765515869354));
#18751=CARTESIAN_POINT('Ctrl Pts',(21.0345534744332,-0.40623841344949,4.15153583326342));
#18752=CARTESIAN_POINT('Ctrl Pts',(21.0584113924646,-0.429177699343215,
3.93836186909709));
#18753=CARTESIAN_POINT('Ctrl Pts',(21.082269310496,-0.347171348131155,3.74026010679315));
#18754=CARTESIAN_POINT('Ctrl Pts',(21.1061272285274,-0.180272145040548,
3.605671823621));
#18755=CARTESIAN_POINT('Ctrl Pts',(21.1299851465589,0.0307085077608185,
3.56750752082027));
#18756=CARTESIAN_POINT('Ctrl Pts',(21.1538430645903,0.234180094072738,3.63509941005724));
#18757=CARTESIAN_POINT('Ctrl Pts',(21.1777009826217,0.380388268371489,3.79191943321731));
#18758=CARTESIAN_POINT('Ctrl Pts',(21.2015589006531,0.433581149524578,3.99962082296209));
#18759=CARTESIAN_POINT('Ctrl Pts',(21.2254168186846,0.380751629084578,4.2074149318183));
#18760=CARTESIAN_POINT('Ctrl Pts',(21.2492747367159,0.234817963878357,4.36449043997717));
#18761=CARTESIAN_POINT('Ctrl Pts',(21.2663360158473,0.0893960873046664,
4.41308118928586));
#18762=CARTESIAN_POINT('Ctrl Pts',(21.2754446556348,0.0100763257733538,
4.41590289708112));
#18763=CARTESIAN_POINT('Ctrl Pts',(21.2766006560785,8.97713258955941E-6,
4.41589335210553));
#18764=CARTESIAN_POINT('Ctrl Pts',(21.0733993439214,-7.65157297121996E-6,
4.41584853425778));
#18765=CARTESIAN_POINT('Ctrl Pts',(21.0763428631935,-0.0256500457845501,
4.41586537097631));
#18766=CARTESIAN_POINT('Ctrl Pts',(21.0872390218095,-0.120560449820324,
4.40722571769055));
#18767=CARTESIAN_POINT('Ctrl Pts',(21.1060878197692,-0.274189543318984,
4.33587624407661));
#18768=CARTESIAN_POINT('Ctrl Pts',(21.1299457378007,-0.401599180171465,
4.16343456021562));
#18769=CARTESIAN_POINT('Ctrl Pts',(21.1538036558321,-0.430806878168669,
3.95102867450389));
#18770=CARTESIAN_POINT('Ctrl Pts',(21.1776615738635,-0.354670559489406,
3.75059761183336));
#18771=CARTESIAN_POINT('Ctrl Pts',(21.2015194918949,-0.191807627993766,
3.61115222665144));
#18772=CARTESIAN_POINT('Ctrl Pts',(21.2253774099264,0.0179574932869785,
3.56679071405539));
#18773=CARTESIAN_POINT('Ctrl Pts',(21.2492353279577,0.223331518303719,3.62836067225603));
#18774=CARTESIAN_POINT('Ctrl Pts',(21.2730932459892,0.374094903668402,3.78080656934254));
#18775=CARTESIAN_POINT('Ctrl Pts',(21.2969511640206,0.433381894944723,3.98685123093373));
#18776=CARTESIAN_POINT('Ctrl Pts',(21.320809082052,0.386695207821707,4.19611112472705));
#18777=CARTESIAN_POINT('Ctrl Pts',(21.3446670000834,0.245451009020076,4.35741650656472));
#18778=CARTESIAN_POINT('Ctrl Pts',(21.3621970873732,0.0975684711839555,
4.41172139589413));
#18779=CARTESIAN_POINT('Ctrl Pts',(21.3717745353192,0.014161952170494,4.41589543043265));
#18780=CARTESIAN_POINT('Ctrl Pts',(21.3733993439214,1.06214664634605E-5,
4.41588075133303));
#18781=CARTESIAN_POINT('Origin',(3.42660065607856,0.,4.));
#18782=CARTESIAN_POINT('',(20.6766006560786,1.29204965968245E-6,4.41591114679826));
#18783=CARTESIAN_POINT('',(20.7733993439214,3.9567662055099E-6,4.41590779860895));
#18784=CARTESIAN_POINT('',(3.42660065607856,4.87367679877478E-13,4.415875));
#18785=CARTESIAN_POINT('Ctrl Pts',(20.6766006560786,1.29076178055295E-6,
4.41591111076812));
#18786=CARTESIAN_POINT('Ctrl Pts',(20.6766286720397,-0.000242659277546582,
4.41591112051333));
#18787=CARTESIAN_POINT('Ctrl Pts',(20.6846093273446,-0.0697345275278937,
4.41585145172406));
#18788=CARTESIAN_POINT('Ctrl Pts',(20.7005426219933,-0.208420567790133,
4.38020336888205));
#18789=CARTESIAN_POINT('Ctrl Pts',(20.7244005400248,-0.365106210756856,
4.23385701605743));
#18790=CARTESIAN_POINT('Ctrl Pts',(20.7482584580562,-0.432520392530856,
4.03032528343114));
#18791=CARTESIAN_POINT('Ctrl Pts',(20.7721163760876,-0.394167874571092,
3.81937870627435));
#18792=CARTESIAN_POINT('Ctrl Pts',(20.795974294119,-0.259432524437891,3.65259868360638));
#18793=CARTESIAN_POINT('Ctrl Pts',(20.8198322121504,-0.0612578225112809,
3.57076788979259));
#18794=CARTESIAN_POINT('Ctrl Pts',(20.8436901301819,0.151895538690754,3.5938959627232));
#18795=CARTESIAN_POINT('Ctrl Pts',(20.8675480482132,0.327906592802717,3.71632757520176));
#18796=CARTESIAN_POINT('Ctrl Pts',(20.8914059662447,0.423735399567132,3.90812480123879));
#18797=CARTESIAN_POINT('Ctrl Pts',(20.9152638842761,0.415949440063929,4.12238802732943));
#18798=CARTESIAN_POINT('Ctrl Pts',(20.9391218023075,0.30645246920106,4.30672404095661));
#18799=CARTESIAN_POINT('Ctrl Pts',(20.9595673929083,0.148398440326279,4.40042000858165));
#18800=CARTESIAN_POINT('Ctrl Pts',(20.9720603441653,0.0395501167658222,
4.4158270594931));
#18801=CARTESIAN_POINT('Ctrl Pts',(20.9766006560786,-4.48287659652116E-6,
4.41584197426197));
#18802=CARTESIAN_POINT('Ctrl Pts',(20.7733993439214,3.95676620551077E-6,
4.41590779860895));
#18803=CARTESIAN_POINT('Ctrl Pts',(20.7809111910678,-0.0654084660523611,
4.41587519962517));
#18804=CARTESIAN_POINT('Ctrl Pts',(20.7963756775582,-0.200102595337945,
4.3835597345012));
#18805=CARTESIAN_POINT('Ctrl Pts',(20.8197928033922,-0.358062019934396,
4.24450842127602));
#18806=CARTESIAN_POINT('Ctrl Pts',(20.8436507214237,-0.431438726014498,
4.04305074550709));
#18807=CARTESIAN_POINT('Ctrl Pts',(20.867508639455,-0.399316990859146,3.83106596928302));
#18808=CARTESIAN_POINT('Ctrl Pts',(20.8913665574865,-0.269551332195825,
3.66039017609669));
#18809=CARTESIAN_POINT('Ctrl Pts',(20.9152244755179,-0.0738730526583281,
3.57275822989076));
#18810=CARTESIAN_POINT('Ctrl Pts',(20.9390823935493,0.139869212314499,3.58959853735383));
#18811=CARTESIAN_POINT('Ctrl Pts',(20.9629403115807,0.319409638666883,3.70679317993256));
#18812=CARTESIAN_POINT('Ctrl Pts',(20.9867982296122,0.420845711130686,3.8956848776653));
#18813=CARTESIAN_POINT('Ctrl Pts',(21.0106561476436,0.419373541863394,4.11008446384341));
#18814=CARTESIAN_POINT('Ctrl Pts',(21.034514065675,0.315353119032788,4.29756540021079));
#18815=CARTESIAN_POINT('Ctrl Pts',(21.0554284644342,0.156567902793621,4.39812991232556));
#18816=CARTESIAN_POINT('Ctrl Pts',(21.0683902238497,0.0436291721249729,
4.41581988245125));
#18817=CARTESIAN_POINT('Ctrl Pts',(21.0733993439214,-7.65157297121996E-6,
4.41584853425778));
#18818=CARTESIAN_POINT('Origin',(3.42660065607856,0.,4.));
#18819=CARTESIAN_POINT('',(20.3766006560786,0.000383027521040961,4.41597069455794));
#18820=CARTESIAN_POINT('',(20.4733993439214,0.000101608071013781,4.41586489633469));
#18821=CARTESIAN_POINT('',(3.42660065607856,4.87367679877478E-13,4.415875));
#18822=CARTESIAN_POINT('Ctrl Pts',(20.3766006560786,0.000383027521040954,
4.41597069455794));
#18823=CARTESIAN_POINT('Ctrl Pts',(20.3891496392578,-0.108893832387875,
4.41487837761012));
#18824=CARTESIAN_POINT('Ctrl Pts',(20.4176039011246,-0.35839559572325,4.31454223548297));
#18825=CARTESIAN_POINT('Ctrl Pts',(20.4540108023354,-0.457800032585507,
3.97025345815189));
#18826=CARTESIAN_POINT('Ctrl Pts',(20.4858213597105,-0.325993724402262,
3.71529210935379));
#18827=CARTESIAN_POINT('Ctrl Pts',(20.509679277742,-0.15096738523986,3.59329490328468));
#18828=CARTESIAN_POINT('Ctrl Pts',(20.5335371957734,0.0630371972956549,
3.57102347342756));
#18829=CARTESIAN_POINT('Ctrl Pts',(20.5573951138048,0.260511246441404,3.65349437971329));
#18830=CARTESIAN_POINT('Ctrl Pts',(20.5812530318362,0.394877283734959,3.82077798440408));
#18831=CARTESIAN_POINT('Ctrl Pts',(20.6051109498677,0.432370081305563,4.03184236506754));
#18832=CARTESIAN_POINT('Ctrl Pts',(20.6289688678991,0.364303478986858,4.23514367899931));
#18833=CARTESIAN_POINT('Ctrl Pts',(20.6527987699694,0.207251017164088,4.38076243960928));
#18834=CARTESIAN_POINT('Ctrl Pts',(20.6686760326959,0.0690052481014253,
4.41590835422812));
#18835=CARTESIAN_POINT('Ctrl Pts',(20.6766006560786,1.29076178055295E-6,
4.41591111076812));
#18836=CARTESIAN_POINT('Ctrl Pts',(20.4733993439214,0.000101608071013788,
4.4158648963347));
#18837=CARTESIAN_POINT('Ctrl Pts',(20.4775268795984,-0.0359150725839473,
4.41584626969953));
#18838=CARTESIAN_POINT('Ctrl Pts',(20.4896070546192,-0.141401612166324,
4.40227446254147));
#18839=CARTESIAN_POINT('Ctrl Pts',(20.5096398689838,-0.298255971346869,
4.31460392554555));
#18840=CARTESIAN_POINT('Ctrl Pts',(20.5334977870152,-0.412709509332759,
4.13311446574462));
#18841=CARTESIAN_POINT('Ctrl Pts',(20.5573557050466,-0.425936384696969,
3.91915434697803));
#18842=CARTESIAN_POINT('Ctrl Pts',(20.581213623078,-0.335173342752607,3.72492109335083));
#18843=CARTESIAN_POINT('Ctrl Pts',(20.6050715411095,-0.162364888615448,
3.59797442377207));
#18844=CARTESIAN_POINT('Ctrl Pts',(20.6289294591408,0.0501004451364318,
3.56932214892951));
#18845=CARTESIAN_POINT('Ctrl Pts',(20.6527873771723,0.250339089241223,3.64598859455508));
#18846=CARTESIAN_POINT('Ctrl Pts',(20.6766452952037,0.389350172549011,3.80921715950176));
#18847=CARTESIAN_POINT('Ctrl Pts',(20.7005032132352,0.433161330121289,4.01909908002448));
#18848=CARTESIAN_POINT('Ctrl Pts',(20.7243611312665,0.371049143609512,4.22430982617278));
#18849=CARTESIAN_POINT('Ctrl Pts',(20.748219049298,0.218207240773441,4.37467120177868));
#18850=CARTESIAN_POINT('Ctrl Pts',(20.7645651201829,0.0769305199015265,
4.41491906931248));
#18851=CARTESIAN_POINT('Ctrl Pts',(20.772958551724,0.00384233167249433,
4.41590971150433));
#18852=CARTESIAN_POINT('Ctrl Pts',(20.7733993439214,3.95676620551077E-6,
4.41590779860895));
#18853=CARTESIAN_POINT('Origin',(3.42660065607856,0.,4.));
#18854=CARTESIAN_POINT('',(20.0766006560786,-0.000186622634748148,4.41645953600834));
#18855=CARTESIAN_POINT('',(20.1733993439214,-0.000111611226006447,4.41653056081536));
#18856=CARTESIAN_POINT('',(3.42660065607856,4.87367679877478E-13,4.415875));
#18857=CARTESIAN_POINT('Ctrl Pts',(20.0766006560786,-0.000186622634748109,
4.41645953600834));
#18858=CARTESIAN_POINT('Ctrl Pts',(20.0778126884445,-0.0107019642254321,
4.4165186149328));
#18859=CARTESIAN_POINT('Ctrl Pts',(20.0949299994981,-0.159149739060163,
4.41138240526969));
#18860=CARTESIAN_POINT('Ctrl Pts',(20.1279525892393,-0.432744382500041,
4.23375285658289));
#18861=CARTESIAN_POINT('Ctrl Pts',(20.1756684253021,-0.430649333670284,
3.76246031529274));
#18862=CARTESIAN_POINT('Ctrl Pts',(20.223384261365,-0.033136228617316,3.50924504180455));
#18863=CARTESIAN_POINT('Ctrl Pts',(20.2711000974278,0.394908089060633,3.70680919012016));
#18864=CARTESIAN_POINT('Ctrl Pts',(20.3188159334906,0.460110046434968,4.17340395051402));
#18865=CARTESIAN_POINT('Ctrl Pts',(20.3539827863742,0.197028357007358,4.40022211154544));
#18866=CARTESIAN_POINT('Ctrl Pts',(20.3732443605702,0.0296097328916507,
4.416262840815));
#18867=CARTESIAN_POINT('Ctrl Pts',(20.3766006560786,0.000383027521040954,
4.41597069455794));
#18868=CARTESIAN_POINT('Ctrl Pts',(20.1733993439214,-0.000111611226006447,
4.41653056081536));
#18869=CARTESIAN_POINT('Ctrl Pts',(20.1741425681289,-0.00655727229825777,
4.41655465488103));
#18870=CARTESIAN_POINT('Ctrl Pts',(20.190791071024,-0.150919726673813,4.41348743992374));
#18871=CARTESIAN_POINT('Ctrl Pts',(20.2233448526067,-0.425711472830213,
4.24633918020534));
#18872=CARTESIAN_POINT('Ctrl Pts',(20.2710606886696,-0.437384262562023,
3.77535541015343));
#18873=CARTESIAN_POINT('Ctrl Pts',(20.3187765247324,-0.0477164433392854,
3.51022640082505));
#18874=CARTESIAN_POINT('Ctrl Pts',(20.3664923607953,0.386374384143037,3.69571627142296));
#18875=CARTESIAN_POINT('Ctrl Pts',(20.4062555575143,0.45143962727185,4.08165775845481));
#18876=CARTESIAN_POINT('Ctrl Pts',(20.4380661148895,0.291471375703242,4.31996082336987));
#18877=CARTESIAN_POINT('Ctrl Pts',(20.4577964972439,0.136183087716603,4.40372206768731));
#18878=CARTESIAN_POINT('Ctrl Pts',(20.4695742402546,0.0334792813416625,
4.41588215816259));
#18879=CARTESIAN_POINT('Ctrl Pts',(20.4733993439214,0.000101608071013788,
4.4158648963347));
#18880=CARTESIAN_POINT('Origin',(3.42660065607856,0.,4.));
#18881=CARTESIAN_POINT('',(19.7766006560786,-0.000280998963924209,4.41539029291088));
#18882=CARTESIAN_POINT('',(19.8733993439214,-0.000322938566065189,4.41548189938477));
#18883=CARTESIAN_POINT('',(3.42660065607856,4.87367679877478E-13,4.415875));
#18884=CARTESIAN_POINT('Ctrl Pts',(19.7766006560786,-0.000280998963924181,
4.41539029291088));
#18885=CARTESIAN_POINT('Ctrl Pts',(19.7823810163188,-0.0507615353771658,
4.41570272077311));
#18886=CARTESIAN_POINT('Ctrl Pts',(19.8040666552467,-0.23976299482565,4.3837755623668));
#18887=CARTESIAN_POINT('Ctrl Pts',(19.8416575728622,-0.481212499922896,
4.10168523844358));
#18888=CARTESIAN_POINT('Ctrl Pts',(19.8893734089251,-0.345789702982467,
3.65023692191923));
#18889=CARTESIAN_POINT('Ctrl Pts',(19.9370892449879,0.107175910646637,3.51998011832295));
#18890=CARTESIAN_POINT('Ctrl Pts',(19.9848050810508,0.461722480014006,3.83053541934297));
#18891=CARTESIAN_POINT('Ctrl Pts',(20.0313088847476,0.394022427012164,4.28486673161383));
#18892=CARTESIAN_POINT('Ctrl Pts',(20.0619074097569,0.127288937001902,4.4157433330307));
#18893=CARTESIAN_POINT('Ctrl Pts',(20.0766006560786,-0.000186622634748109,
4.41645953600834));
#18894=CARTESIAN_POINT('Ctrl Pts',(19.8733993439214,-0.000322938566065196,
4.41548189938477));
#18895=CARTESIAN_POINT('Ctrl Pts',(19.8787108960032,-0.0466836533228258,
4.41581668875846));
#18896=CARTESIAN_POINT('Ctrl Pts',(19.8999277267727,-0.231469429366377,
4.38724295332581));
#18897=CARTESIAN_POINT('Ctrl Pts',(19.9370498362297,-0.47800980043334,4.11581244897344));
#18898=CARTESIAN_POINT('Ctrl Pts',(19.9847656722926,-0.355939225796451,
3.66057517601247));
#18899=CARTESIAN_POINT('Ctrl Pts',(20.0324815083554,0.0929888682922082,
3.51702731322357));
#18900=CARTESIAN_POINT('Ctrl Pts',(20.0801973444182,0.456536973876988,3.81701888067549));
#18901=CARTESIAN_POINT('Ctrl Pts',(20.1271699562736,0.401683300383188,4.27772103607547));
#18902=CARTESIAN_POINT('Ctrl Pts',(20.1582372894413,0.131382308576697,4.41603903277767));
#18903=CARTESIAN_POINT('Ctrl Pts',(20.1733993439214,-0.000111611226006447,
4.41653056081536));
#18904=CARTESIAN_POINT('Origin',(3.42660065607856,0.,4.));
#18905=CARTESIAN_POINT('',(19.4766006560786,0.000302289446139524,4.41543216566181));
#18906=CARTESIAN_POINT('',(19.5733993439214,0.000255464646300079,4.41534829948978));
#18907=CARTESIAN_POINT('',(3.42660065607856,4.87367679877478E-13,4.415875));
#18908=CARTESIAN_POINT('Ctrl Pts',(19.4766006560786,0.000302289446139546,
4.41543216566181));
#18909=CARTESIAN_POINT('Ctrl Pts',(19.4869493441932,-0.0900510892866153,
4.41482666801407));
#18910=CARTESIAN_POINT('Ctrl Pts',(19.5132033109954,-0.320168095705801,
4.3413809155508));
#18911=CARTESIAN_POINT('Ctrl Pts',(19.5553625564852,-0.490312813065352,
3.96128857502183));
#18912=CARTESIAN_POINT('Ctrl Pts',(19.603078392548,-0.232620797759261,3.56664935826393));
#18913=CARTESIAN_POINT('Ctrl Pts',(19.6507942286109,0.238690449241969,3.56996267500769));
#18914=CARTESIAN_POINT('Ctrl Pts',(19.6985100646737,0.490808633485035,3.96818593857384));
#18915=CARTESIAN_POINT('Ctrl Pts',(19.7404455404963,0.316268156276861,4.34384396940031));
#18916=CARTESIAN_POINT('Ctrl Pts',(19.7664757376312,0.0881410531427697,
4.41484304213512));
#18917=CARTESIAN_POINT('Ctrl Pts',(19.7766006560786,-0.000280998963924181,
4.41539029291088));
#18918=CARTESIAN_POINT('Ctrl Pts',(19.5733993439214,0.000255464646300094,
4.41534829948978));
#18919=CARTESIAN_POINT('Ctrl Pts',(19.5832792238775,-0.0860485087386658,
4.41486588036018));
#18920=CARTESIAN_POINT('Ctrl Pts',(19.6090643825213,-0.311990568344336,
4.34649332259355));
#18921=CARTESIAN_POINT('Ctrl Pts',(19.6507548198527,-0.491240257057309,
3.97574594767572));
#18922=CARTESIAN_POINT('Ctrl Pts',(19.6984706559155,-0.245282818621706,
3.57368850533185));
#18923=CARTESIAN_POINT('Ctrl Pts',(19.7461864919783,0.225921452997342,3.56311925573479));
#18924=CARTESIAN_POINT('Ctrl Pts',(19.7939023280412,0.489658867576397,3.95374471702426));
#18925=CARTESIAN_POINT('Ctrl Pts',(19.8363066120222,0.324430886710512,4.33863507066385));
#18926=CARTESIAN_POINT('Ctrl Pts',(19.8628056173156,0.0921420753912029,
4.4148141723173));
#18927=CARTESIAN_POINT('Ctrl Pts',(19.8733993439214,-0.000322938566065196,
4.41548189938477));
#18928=CARTESIAN_POINT('Origin',(3.42660065607856,0.,4.));
#18929=CARTESIAN_POINT('',(19.1766006560786,0.000155842099650094,4.41649089206047));
#18930=CARTESIAN_POINT('',(19.2733993439214,0.000220989830587742,4.4164164649367));
#18931=CARTESIAN_POINT('',(3.42660065607856,4.87367679877478E-13,4.415875));
#18932=CARTESIAN_POINT('Ctrl Pts',(19.1766006560786,0.000155842099650088,
4.41649089206047));
#18933=CARTESIAN_POINT('Ctrl Pts',(19.1915176720675,-0.129233580897558,
4.41587069825202));
#18934=CARTESIAN_POINT('Ctrl Pts',(19.2223399667441,-0.397695790553126,
4.28149179527637));
#18935=CARTESIAN_POINT('Ctrl Pts',(19.2690675401082,-0.459293044881286,
3.82405931712685));
#18936=CARTESIAN_POINT('Ctrl Pts',(19.316783376171,-0.100417177000157,3.51852142809106));
#18937=CARTESIAN_POINT('Ctrl Pts',(19.3644992122339,0.350673329058588,3.65513271950473));
#18938=CARTESIAN_POINT('Ctrl Pts',(19.4122150482967,0.479735122332443,4.10844094226069));
#18939=CARTESIAN_POINT('Ctrl Pts',(19.4495821962449,0.235804435834584,4.38544967282755));
#18940=CARTESIAN_POINT('Ctrl Pts',(19.4710440655056,0.0488163355692654,
4.4157572795781));
#18941=CARTESIAN_POINT('Ctrl Pts',(19.4766006560786,0.000302289446139546,
4.41543216566181));
#18942=CARTESIAN_POINT('Ctrl Pts',(19.2733993439214,0.000220989830587761,
4.4164164649367));
#18943=CARTESIAN_POINT('Ctrl Pts',(19.2878475517519,-0.125161313229646,
4.41561068768233));
#18944=CARTESIAN_POINT('Ctrl Pts',(19.31820103827,-0.389985711500173,4.28851341748863));
#18945=CARTESIAN_POINT('Ctrl Pts',(19.3644598034757,-0.464275578741542,
3.8376626582024));
#18946=CARTESIAN_POINT('Ctrl Pts',(19.4121756395385,-0.114554038379521,
3.52168776344319));
#18947=CARTESIAN_POINT('Ctrl Pts',(19.4598914756013,0.340364234683876,3.64495435060606));
#18948=CARTESIAN_POINT('Ctrl Pts',(19.5076073116642,0.482720800247919,4.09426482953845));
#18949=CARTESIAN_POINT('Ctrl Pts',(19.5454432677708,0.244097666198316,4.38190156491584));
#18950=CARTESIAN_POINT('Ctrl Pts',(19.5673739451899,0.0528892875329133,
4.41564251031262));
#18951=CARTESIAN_POINT('Ctrl Pts',(19.5733993439214,0.000255464646300094,
4.41534829948978));
#18952=CARTESIAN_POINT('Origin',(3.42660065607856,0.,4.));
#18953=CARTESIAN_POINT('',(18.8766006560785,-0.00038196507782994,4.41590683121974));
#18954=CARTESIAN_POINT('',(18.9733993439214,-0.000368287616214491,4.41603142687637));
#18955=CARTESIAN_POINT('',(3.42660065607856,4.87367679877478E-13,4.415875));
#18956=CARTESIAN_POINT('Ctrl Pts',(18.8766006560785,-0.000381965077829925,
4.41590683121974));
#18957=CARTESIAN_POINT('Ctrl Pts',(18.8801807212542,-0.0315488007868432,
4.41619587167324));
#18958=CARTESIAN_POINT('Ctrl Pts',(18.8996660651174,-0.200861076696893,
4.39874895857547));
#18959=CARTESIAN_POINT('Ctrl Pts',(18.9350566876684,-0.462607878309702,
4.16703046362027));
#18960=CARTESIAN_POINT('Ctrl Pts',(18.9827725237311,-0.39069124519864,3.70122654773242));
#18961=CARTESIAN_POINT('Ctrl Pts',(19.030488359794,0.0400031699426168,3.50979089028978));
#18962=CARTESIAN_POINT('Ctrl Pts',(19.0782041958568,0.433962058584907,3.76852180111673));
#18963=CARTESIAN_POINT('Ctrl Pts',(19.1259200319197,0.429406911488226,4.23982270375453));
#18964=CARTESIAN_POINT('Ctrl Pts',(19.1587188519936,0.155221332864305,4.41240136130926));
#18965=CARTESIAN_POINT('Ctrl Pts',(19.1756123933799,0.00872798149047904,
4.41653198033223));
#18966=CARTESIAN_POINT('Ctrl Pts',(19.1766006560786,0.000155842099650088,
4.41649089206047));
#18967=CARTESIAN_POINT('Ctrl Pts',(18.9733993439214,-0.000368287616214533,
4.41603142687637));
#18968=CARTESIAN_POINT('Ctrl Pts',(18.9765106009386,-0.0274330213022572,
4.4162811262788));
#18969=CARTESIAN_POINT('Ctrl Pts',(18.9955271366434,-0.192586232161443,
4.40152565608163));
#18970=CARTESIAN_POINT('Ctrl Pts',(19.0304489510358,-0.457487847288108,
4.18058265263639));
#18971=CARTESIAN_POINT('Ctrl Pts',(19.0781647870987,-0.399321187381313,
3.71286272589862));
#18972=CARTESIAN_POINT('Ctrl Pts',(19.1258806231614,0.0255482632835279,
3.50882537619781));
#18973=CARTESIAN_POINT('Ctrl Pts',(19.1735964592243,0.426956350589889,3.75584124112414));
#18974=CARTESIAN_POINT('Ctrl Pts',(19.2213122952871,0.436283851722622,4.22707185138688));
#18975=CARTESIAN_POINT('Ctrl Pts',(19.2545799235195,0.163455264474221,4.41023200720537));
#18976=CARTESIAN_POINT('Ctrl Pts',(19.2719422730642,0.0128655269200745,
4.41649772584937));
#18977=CARTESIAN_POINT('Ctrl Pts',(19.2733993439214,0.000220989830587761,
4.4164164649367));
#18978=CARTESIAN_POINT('Origin',(3.42660065607856,0.,4.));
#18979=CARTESIAN_POINT('',(18.5766006560786,2.82854505807383E-5,4.41518799822097));
#18980=CARTESIAN_POINT('',(18.6733993439214,-3.94222854199766E-5,4.41518963037823));
#18981=CARTESIAN_POINT('',(3.42660065607856,4.87367679877478E-13,4.415875));
#18982=CARTESIAN_POINT('Ctrl Pts',(18.5766006560786,2.82854505807215E-5,
4.41518799822097));
#18983=CARTESIAN_POINT('Ctrl Pts',(18.5847490491285,-0.0712192880865648,
4.41514491699706));
#18984=CARTESIAN_POINT('Ctrl Pts',(18.6088027208661,-0.281596950705947,
4.36382162423513));
#18985=CARTESIAN_POINT('Ctrl Pts',(18.6487616712913,-0.49096944006335,4.0292272779409));
#18986=CARTESIAN_POINT('Ctrl Pts',(18.6964775073541,-0.290120809601049,
3.60284116440841));
#18987=CARTESIAN_POINT('Ctrl Pts',(18.744193343417,0.177150224400508,3.54117212067402));
#18988=CARTESIAN_POINT('Ctrl Pts',(18.7919091794797,0.481741481528227,3.90085177849878));
#18989=CARTESIAN_POINT('Ctrl Pts',(18.836044950367,0.354281053487698,4.31776308733785));
#18990=CARTESIAN_POINT('Ctrl Pts',(18.8642754425666,0.106917172161326,4.4149117417093));
#18991=CARTESIAN_POINT('Ctrl Pts',(18.8766006560785,-0.000381965077829925,
4.41590683121974));
#18992=CARTESIAN_POINT('Ctrl Pts',(18.6733993439214,-3.94222854199489E-5,
4.41518963037823));
#18993=CARTESIAN_POINT('Ctrl Pts',(18.6810789288129,-0.0671871929144198,
4.41524623173262));
#18994=CARTESIAN_POINT('Ctrl Pts',(18.704663792392,-0.273330541024821,4.36810584919535));
#18995=CARTESIAN_POINT('Ctrl Pts',(18.7441539346588,-0.489895661254576,
4.0436745456279));
#18996=CARTESIAN_POINT('Ctrl Pts',(18.7918697707216,-0.301692008317894,
3.6115580391236));
#18997=CARTESIAN_POINT('Ctrl Pts',(18.8395856067845,0.163560057986223,3.53615376224111));
#18998=CARTESIAN_POINT('Ctrl Pts',(18.8873014428472,0.478612406344963,3.88670662268212));
#18999=CARTESIAN_POINT('Ctrl Pts',(18.9319060218929,0.362263203066427,4.31165738429376));
#19000=CARTESIAN_POINT('Ctrl Pts',(18.960605322251,0.110926532249199,4.41500462017153));
#19001=CARTESIAN_POINT('Ctrl Pts',(18.9733993439214,-0.000368287616214533,
4.41603142687637));
#19002=CARTESIAN_POINT('Origin',(3.42660065607856,0.,4.));
#19003=CARTESIAN_POINT('',(18.2766006560786,0.000371443240938316,4.41601098728712));
#19004=CARTESIAN_POINT('',(18.3733993439214,0.000382963303967143,4.41588626824893));
#19005=CARTESIAN_POINT('',(3.42660065607856,4.87367679877478E-13,4.415875));
#19006=CARTESIAN_POINT('Ctrl Pts',(18.2766006560785,0.000371443240938293,
4.41601098728712));
#19007=CARTESIAN_POINT('Ctrl Pts',(18.2893173770028,-0.110264925490287,
4.41498710445335));
#19008=CARTESIAN_POINT('Ctrl Pts',(18.3179393766147,-0.360950442388199,
4.31267773405576));
#19009=CARTESIAN_POINT('Ctrl Pts',(18.3624666549143,-0.479157019140895,
3.88903254594255));
#19010=CARTESIAN_POINT('Ctrl Pts',(18.4101824909771,-0.165810997523729,
3.5369536330429));
#19011=CARTESIAN_POINT('Ctrl Pts',(18.4578983270399,0.299801814449608,3.61009732380414));
#19012=CARTESIAN_POINT('Ctrl Pts',(18.5056141631028,0.49010200717001,4.04129464153984));
#19013=CARTESIAN_POINT('Ctrl Pts',(18.5451816061157,0.274694351318236,4.36741107590602));
#19014=CARTESIAN_POINT('Ctrl Pts',(18.5688437704409,0.0678526130816757,
4.41522900951301));
#19015=CARTESIAN_POINT('Ctrl Pts',(18.5766006560786,2.82854505807215E-5,
4.41518799822097));
#19016=CARTESIAN_POINT('Ctrl Pts',(18.3733993439214,0.000382963303967157,
4.41588626824893));
#19017=CARTESIAN_POINT('Ctrl Pts',(18.3856472566872,-0.106256708375174,
4.41489942083623));
#19018=CARTESIAN_POINT('Ctrl Pts',(18.4138004481407,-0.352960303644862,
4.31875095920395));
#19019=CARTESIAN_POINT('Ctrl Pts',(18.4578589182817,-0.482217355384067,
3.90319273261591));
#19020=CARTESIAN_POINT('Ctrl Pts',(18.5055747543446,-0.179376629827252,
3.54203793877243));
#19021=CARTESIAN_POINT('Ctrl Pts',(18.5532905904074,0.288188414964166,3.60143675240633));
#19022=CARTESIAN_POINT('Ctrl Pts',(18.6010064264702,0.491105603945206,4.02684232898929));
#19023=CARTESIAN_POINT('Ctrl Pts',(18.6410426776416,0.282958802096416,4.36309886994028));
#19024=CARTESIAN_POINT('Ctrl Pts',(18.6651736501253,0.0718833454275778,
4.41512900400112));
#19025=CARTESIAN_POINT('Ctrl Pts',(18.6733993439214,-3.94222854199489E-5,
4.41518963037823));
#19026=CARTESIAN_POINT('Origin',(3.42660065607856,0.,4.));
#19027=CARTESIAN_POINT('',(17.9766006560786,-0.000210814279110197,4.41643020456723));
#19028=CARTESIAN_POINT('',(18.0733993439214,-0.000144384975211464,4.41650095473263));
#19029=CARTESIAN_POINT('',(3.42660065607856,4.87367679877478E-13,4.415875));
#19030=CARTESIAN_POINT('Ctrl Pts',(17.9766006560786,-0.000210814279110157,
4.41643020456723));
#19031=CARTESIAN_POINT('Ctrl Pts',(17.9779804261896,-0.0121834889824064,
4.41650424974197));
#19032=CARTESIAN_POINT('Ctrl Pts',(17.9952654749882,-0.162096873242269,
4.41059855206721));
#19033=CARTESIAN_POINT('Ctrl Pts',(18.0284558024744,-0.435175833605105,
4.22918817311999));
#19034=CARTESIAN_POINT('Ctrl Pts',(18.0761716385373,-0.428137176707308,
3.75791781814212));
#19035=CARTESIAN_POINT('Ctrl Pts',(18.1238874746,-0.0279335627019553,3.5089552556775));
#19036=CARTESIAN_POINT('Ctrl Pts',(18.1716033106629,0.397921871745719,3.71092663761881));
#19037=CARTESIAN_POINT('Ctrl Pts',(18.2193191467257,0.458359528554279,4.17835853620019));
#19038=CARTESIAN_POINT('Ctrl Pts',(18.2543182618643,0.193950155243433,4.40107745006558));
#19039=CARTESIAN_POINT('Ctrl Pts',(18.2734120983152,0.0281121206155762,
4.41626771302466));
#19040=CARTESIAN_POINT('Ctrl Pts',(18.2766006560785,0.000371443240938293,
4.41601098728712));
#19041=CARTESIAN_POINT('Ctrl Pts',(18.0733993439214,-0.000144384975211439,
4.41650095473263));
#19042=CARTESIAN_POINT('Ctrl Pts',(18.0743103058739,-0.00804551399413891,
4.41653639380418));
#19043=CARTESIAN_POINT('Ctrl Pts',(18.0911265465141,-0.153864670001157,
4.41274680364665));
#19044=CARTESIAN_POINT('Ctrl Pts',(18.1238480658419,-0.428237044548737,
4.24190547436581));
#19045=CARTESIAN_POINT('Ctrl Pts',(18.1715639019047,-0.435081213444543,
3.7706322547532));
#19046=CARTESIAN_POINT('Ctrl Pts',(18.2192797379675,-0.0423836094492617,
3.50999096487715));
#19047=CARTESIAN_POINT('Ctrl Pts',(18.2669955740304,0.389235515258945,3.69933251171255));
#19048=CARTESIAN_POINT('Ctrl Pts',(18.3147114100932,0.463413677146622,4.16478163940629));
#19049=CARTESIAN_POINT('Ctrl Pts',(18.3501793333902,0.202226156869028,4.39827758107438));
#19050=CARTESIAN_POINT('Ctrl Pts',(18.3697419779996,0.0322267809866215,
4.41618095209965));
#19051=CARTESIAN_POINT('Ctrl Pts',(18.3733993439214,0.000382963303967157,
4.41588626824893));
#19052=CARTESIAN_POINT('Origin',(3.42660065607856,0.,4.));
#19053=CARTESIAN_POINT('',(17.6766006560786,-0.000263771022561219,4.41536107794487));
#19054=CARTESIAN_POINT('',(17.7733993439214,-0.000309142357869163,4.41544738986064));
#19055=CARTESIAN_POINT('',(3.42660065607856,4.87367679877478E-13,4.415875));
#19056=CARTESIAN_POINT('Ctrl Pts',(17.6766006560786,-0.000263771022561289,
4.41536107794487));
#19057=CARTESIAN_POINT('Ctrl Pts',(17.6825487540639,-0.0522183410383149,
4.41566152300153));
#19058=CARTESIAN_POINT('Ctrl Pts',(17.7044021307368,-0.24273028972288,4.38249735042552));
#19059=CARTESIAN_POINT('Ctrl Pts',(17.7421607860973,-0.48225726547346,4.09660825404716));
#19060=CARTESIAN_POINT('Ctrl Pts',(17.7898766221602,-0.342084653792828,
3.64661166616396));
#19061=CARTESIAN_POINT('Ctrl Pts',(17.837592458223,0.112229559114723,3.52113702282083));
#19062=CARTESIAN_POINT('Ctrl Pts',(17.8853082942859,0.463481641013499,3.83540961967535));
#19063=CARTESIAN_POINT('Ctrl Pts',(17.9316443602377,0.391261919872151,4.28736986940801));
#19064=CARTESIAN_POINT('Ctrl Pts',(17.962075147502,0.125831334120538,4.41565069513148));
#19065=CARTESIAN_POINT('Ctrl Pts',(17.9766006560786,-0.000210814279110157,
4.41643020456723));
#19066=CARTESIAN_POINT('Ctrl Pts',(17.7733993439214,-0.000309142357869142,
4.41544738986064));
#19067=CARTESIAN_POINT('Ctrl Pts',(17.7788786337482,-0.0481438769258273,
4.41577602216682));
#19068=CARTESIAN_POINT('Ctrl Pts',(17.8002632022627,-0.23443694547481,4.38601982759396));
#19069=CARTESIAN_POINT('Ctrl Pts',(17.8375530494648,-0.479202773223469,
4.11076970247734));
#19070=CARTESIAN_POINT('Ctrl Pts',(17.8852688855277,-0.352344189444135,
3.65683998336499));
#19071=CARTESIAN_POINT('Ctrl Pts',(17.9329847215905,0.0980774850139738,
3.51803938772416));
#19072=CARTESIAN_POINT('Ctrl Pts',(17.9807005576534,0.458433095867658,3.82183063825345));
#19073=CARTESIAN_POINT('Ctrl Pts',(18.0275054317636,0.3989600628602,4.28031410431705));
#19074=CARTESIAN_POINT('Ctrl Pts',(18.0584050271863,0.129907183855675,4.41591763216682));
#19075=CARTESIAN_POINT('Ctrl Pts',(18.0733993439214,-0.000144384975211439,
4.41650095473263));
#19076=CARTESIAN_POINT('Origin',(3.42660065607856,0.,4.));
#19077=CARTESIAN_POINT('',(17.3766006560786,0.000316824918469052,4.41546566829253));
#19078=CARTESIAN_POINT('',(17.4733993439214,0.000273208168652644,4.41537657040552));
#19079=CARTESIAN_POINT('',(3.42660065607856,4.87367679877478E-13,4.415875));
#19080=CARTESIAN_POINT('Ctrl Pts',(17.3766006560786,0.000316824918469058,
4.41546566829253));
#19081=CARTESIAN_POINT('Ctrl Pts',(17.3871170819382,-0.0914824399419538,
4.4148173972429));
#19082=CARTESIAN_POINT('Ctrl Pts',(17.4135387864855,-0.323087181591141,
4.33950699049548));
#19083=CARTESIAN_POINT('Ctrl Pts',(17.4558657697204,-0.489877595596684,
3.956123284257));
#19084=CARTESIAN_POINT('Ctrl Pts',(17.5035816057832,-0.228040769637767,
3.56422180844494));
#19085=CARTESIAN_POINT('Ctrl Pts',(17.551297441846,0.243209403937772,3.57250215124727));
#19086=CARTESIAN_POINT('Ctrl Pts',(17.5990132779089,0.491116639619549,3.97336034645914));
#19087=CARTESIAN_POINT('Ctrl Pts',(17.6407810159864,0.313340775136121,4.34566293955037));
#19088=CARTESIAN_POINT('Ctrl Pts',(17.6666434753763,0.0867087440962768,
4.41485812965324));
#19089=CARTESIAN_POINT('Ctrl Pts',(17.6766006560786,-0.000263771022561289,
4.41536107794487));
#19090=CARTESIAN_POINT('Ctrl Pts',(17.4733993439214,0.000273208168652693,
4.41537657040552));
#19091=CARTESIAN_POINT('Ctrl Pts',(17.4834469616226,-0.0874810350323011,
4.41484969107387));
#19092=CARTESIAN_POINT('Ctrl Pts',(17.5093998580114,-0.314919534962053,
4.34468516187688));
#19093=CARTESIAN_POINT('Ctrl Pts',(17.5512580330878,-0.490957336521241,
3.97057010757845));
#19094=CARTESIAN_POINT('Ctrl Pts',(17.5989738691507,-0.240776309167652,
3.57112706567612));
#19095=CARTESIAN_POINT('Ctrl Pts',(17.6466897052135,0.230513307714322,3.56552463842171));
#19096=CARTESIAN_POINT('Ctrl Pts',(17.6944055412763,0.490119007219086,3.95890762096741));
#19097=CARTESIAN_POINT('Ctrl Pts',(17.7366420875123,0.321513805022658,4.34052027563639));
#19098=CARTESIAN_POINT('Ctrl Pts',(17.7629733550606,0.090710757213051,4.41482206853766));
#19099=CARTESIAN_POINT('Ctrl Pts',(17.7733993439214,-0.000309142357869142,
4.41544738986064));
#19100=CARTESIAN_POINT('Origin',(3.42660065607856,0.,4.));
#19101=CARTESIAN_POINT('',(17.0766006560786,0.000130763213737631,4.41651185352269));
#19102=CARTESIAN_POINT('',(17.1733993439214,0.000198609043858391,4.41644558073401));
#19103=CARTESIAN_POINT('',(3.42660065607856,4.87367679877478E-13,4.415875));
#19104=CARTESIAN_POINT('Ctrl Pts',(17.0766006560786,0.000130763213737628,
4.41651185352269));
#19105=CARTESIAN_POINT('Ctrl Pts',(17.0916854098125,-0.130696083011285,
4.41597403242798));
#19106=CARTESIAN_POINT('Ctrl Pts',(17.1226754422341,-0.400436570105288,
4.2789290971087));
#19107=CARTESIAN_POINT('Ctrl Pts',(17.1695707533433,-0.457413284126125,
3.81922856321607));
#19108=CARTESIAN_POINT('Ctrl Pts',(17.2172865894061,-0.0953372598908034,
3.51748986360026));
#19109=CARTESIAN_POINT('Ctrl Pts',(17.265002425469,0.354288437054553,3.6588476466131));
#19110=CARTESIAN_POINT('Ctrl Pts',(17.3127182615318,0.478565610824392,4.11349088504481));
#19111=CARTESIAN_POINT('Ctrl Pts',(17.349917671735,0.232837083242772,4.38668157013213));
#19112=CARTESIAN_POINT('Ctrl Pts',(17.3712118032506,0.0473568302064652,
4.41579785693967));
#19113=CARTESIAN_POINT('Ctrl Pts',(17.3766006560786,0.000316824918469058,
4.41546566829253));
#19114=CARTESIAN_POINT('Ctrl Pts',(17.1733993439214,0.000198609043858397,
4.41644558073401));
#19115=CARTESIAN_POINT('Ctrl Pts',(17.1880152894969,-0.126615914365149,
4.41569892234974));
#19116=CARTESIAN_POINT('Ctrl Pts',(17.2185365137601,-0.392752582168809,
4.28602487069057));
#19117=CARTESIAN_POINT('Ctrl Pts',(17.2649630167107,-0.462538907526291,
3.83277863809798));
#19118=CARTESIAN_POINT('Ctrl Pts',(17.3126788527736,-0.109506707187599,
3.52050703244687));
#19119=CARTESIAN_POINT('Ctrl Pts',(17.3603946888365,0.344087187338735,3.64856119684745));
#19120=CARTESIAN_POINT('Ctrl Pts',(17.4081105248993,0.481700523269991,4.09934702176407));
#19121=CARTESIAN_POINT('Ctrl Pts',(17.4457787432609,0.241130489326423,4.3831889686244));
#19122=CARTESIAN_POINT('Ctrl Pts',(17.467541682935,0.0514330574063097,4.41568373580506));
#19123=CARTESIAN_POINT('Ctrl Pts',(17.4733993439214,0.000273208168652693,
4.41537657040552));
#19124=CARTESIAN_POINT('Origin',(3.42660065607856,0.,4.));
#19125=CARTESIAN_POINT('',(16.7766006560786,-0.000383680820852129,4.41586226484778));
#19126=CARTESIAN_POINT('',(16.8733993439214,-0.000374684679869397,4.41598699190495));
#19127=CARTESIAN_POINT('',(3.42660065607856,4.87367679877478E-13,4.415875));
#19128=CARTESIAN_POINT('Ctrl Pts',(16.7766006560786,-0.000383680820852189,
4.41586226484779));
#19129=CARTESIAN_POINT('Ctrl Pts',(16.7803484589992,-0.0330197262611539,
4.41616320579436));
#19130=CARTESIAN_POINT('Ctrl Pts',(16.8000015406075,-0.203823433586872,
4.39772119122577));
#19131=CARTESIAN_POINT('Ctrl Pts',(16.8355599009034,-0.464342533291602,
4.16214572651883));
#19132=CARTESIAN_POINT('Ctrl Pts',(16.8832757369663,-0.387520750342007,
3.69712561530174));
#19133=CARTESIAN_POINT('Ctrl Pts',(16.9309915730291,0.0451673004198413,
3.51023971187451));
#19134=CARTESIAN_POINT('Ctrl Pts',(16.978707409092,0.436377524217892,3.7731082169636));
#19135=CARTESIAN_POINT('Ctrl Pts',(17.0264232451548,0.426855552995382,4.24433493759383));
#19136=CARTESIAN_POINT('Ctrl Pts',(17.0590543274837,0.152277829190936,4.41314658311127));
#19137=CARTESIAN_POINT('Ctrl Pts',(17.0757801311249,0.00724700082869906,
4.41654110793655));
#19138=CARTESIAN_POINT('Ctrl Pts',(17.0766006560786,0.000130763213737628,
4.41651185352269));
#19139=CARTESIAN_POINT('Ctrl Pts',(16.8733993439214,-0.000374684679869387,
4.41598699190495));
#19140=CARTESIAN_POINT('Ctrl Pts',(16.8766783386836,-0.0289064002234668,
4.4162516892709));
#19141=CARTESIAN_POINT('Ctrl Pts',(16.8958626121335,-0.195546116663039,
4.40054826733105));
#19142=CARTESIAN_POINT('Ctrl Pts',(16.9309521642709,-0.459365614209645,
4.17575112327883));
#19143=CARTESIAN_POINT('Ctrl Pts',(16.9786680003337,-0.396272847821079,
3.70867019559999));
#19144=CARTESIAN_POINT('Ctrl Pts',(17.0263838363966,0.0307233721630972,
3.5091219099869));
#19145=CARTESIAN_POINT('Ctrl Pts',(17.0740996724594,0.429505846750062,3.76035452756312));
#19146=CARTESIAN_POINT('Ctrl Pts',(17.1218155085223,0.433866493469502,4.23165726989771));
#19147=CARTESIAN_POINT('Ctrl Pts',(17.1549153990096,0.160507997039396,4.41102293437065));
#19148=CARTESIAN_POINT('Ctrl Pts',(17.1721100108093,0.0113854435377776,
4.41651144656345));
#19149=CARTESIAN_POINT('Ctrl Pts',(17.1733993439214,0.000198609043858397,
4.41644558073401));
#19150=CARTESIAN_POINT('Origin',(3.42660065607856,0.,4.));
#19151=CARTESIAN_POINT('',(16.4766006560786,5.2409936866527E-5,4.41519222098806));
#19152=CARTESIAN_POINT('',(16.5733993439214,-1.52272386678698E-5,4.41518677123726));
#19153=CARTESIAN_POINT('',(3.42660065607856,4.87367679877478E-13,4.415875));
#19154=CARTESIAN_POINT('Ctrl Pts',(16.4766006560786,5.2409936866539E-5,
4.41519222098806));
#19155=CARTESIAN_POINT('Ctrl Pts',(16.4849167868736,-0.0726599781719204,
4.41511070701236));
#19156=CARTESIAN_POINT('Ctrl Pts',(16.5091381963562,-0.284551613766983,
4.36224737480062));
#19157=CARTESIAN_POINT('Ctrl Pts',(16.5492648845264,-0.4912502013546,4.02405128938415));
#19158=CARTESIAN_POINT('Ctrl Pts',(16.5969807205893,-0.285919008936969,
3.59980561575594));
#19159=CARTESIAN_POINT('Ctrl Pts',(16.6446965566521,0.181976008816936,3.54306460296116));
#19160=CARTESIAN_POINT('Ctrl Pts',(16.6924123927149,0.482759657613431,3.90593439612197));
#19161=CARTESIAN_POINT('Ctrl Pts',(16.7363804258571,0.351413532087107,4.31989995948535));
#19162=CARTESIAN_POINT('Ctrl Pts',(16.7644431803116,0.105484194296011,4.41488604428797));
#19163=CARTESIAN_POINT('Ctrl Pts',(16.7766006560786,-0.000383680820852189,
4.41586226484779));
#19164=CARTESIAN_POINT('Ctrl Pts',(16.5733993439214,-1.52272386678906E-5,
4.41518677123726));
#19165=CARTESIAN_POINT('Ctrl Pts',(16.5812466665579,-0.0686308195205231,
4.41520910309265));
#19166=CARTESIAN_POINT('Ctrl Pts',(16.6049992678821,-0.276289552895371,
4.36659242126669));
#19167=CARTESIAN_POINT('Ctrl Pts',(16.6446571478939,-0.490328743065594,
4.03850907134293));
#19168=CARTESIAN_POINT('Ctrl Pts',(16.6923729839567,-0.297581432841348,
3.60840005658827));
#19169=CARTESIAN_POINT('Ctrl Pts',(16.7400888200196,0.168439486040012,3.53790329540825));
#19170=CARTESIAN_POINT('Ctrl Pts',(16.7878046560824,0.479779833116189,3.89175704832657));
#19171=CARTESIAN_POINT('Ctrl Pts',(16.832241497383,0.359412856911567,4.31386464726761));
#19172=CARTESIAN_POINT('Ctrl Pts',(16.860773059996,0.109491163683573,4.41496773315674));
#19173=CARTESIAN_POINT('Ctrl Pts',(16.8733993439214,-0.000374684679869387,
4.41598699190495));
#19174=CARTESIAN_POINT('Origin',(3.42660065607856,0.,4.));
#19175=CARTESIAN_POINT('',(16.1766006560786,0.000364146841390381,4.41605523138122));
#19176=CARTESIAN_POINT('',(16.2733993439214,0.000380345806842055,4.41593091837313));
#19177=CARTESIAN_POINT('',(3.42660065607856,4.87367679877478E-13,4.415875));
#19178=CARTESIAN_POINT('Ctrl Pts',(16.1766006560786,0.000364146841390366,
4.41605523138122));
#19179=CARTESIAN_POINT('Ctrl Pts',(16.1894851147479,-0.111700864104492,
4.41502624848758));
#19180=CARTESIAN_POINT('Ctrl Pts',(16.2182748521048,-0.363797281821349,
4.31045679267864));
#19181=CARTESIAN_POINT('Ctrl Pts',(16.2629698681494,-0.477960913216358,
3.88398883549692));
#19182=CARTESIAN_POINT('Ctrl Pts',(16.3106857042122,-0.160921706883503,
3.53523185446324));
#19183=CARTESIAN_POINT('Ctrl Pts',(16.358401540275,0.303894378979202,3.6132786128531));
#19184=CARTESIAN_POINT('Ctrl Pts',(16.4061173763379,0.489639580609251,4.04645757153336));
#19185=CARTESIAN_POINT('Ctrl Pts',(16.4455170816057,0.271734615807756,4.36891289568356));
#19186=CARTESIAN_POINT('Ctrl Pts',(16.4690115081859,0.0664083969439258,
4.41526660914191));
#19187=CARTESIAN_POINT('Ctrl Pts',(16.4766006560786,5.2409936866539E-5,
4.41519222098806));
#19188=CARTESIAN_POINT('Ctrl Pts',(16.2733993439214,0.000380345806842052,
4.41593091837313));
#19189=CARTESIAN_POINT('Ctrl Pts',(16.2858149944323,-0.107690075887363,
4.41492720978183));
#19190=CARTESIAN_POINT('Ctrl Pts',(16.3141359236307,-0.35582464097624,4.31660057631701));
#19191=CARTESIAN_POINT('Ctrl Pts',(16.3583621315169,-0.481170314810987,
3.89811598262401));
#19192=CARTESIAN_POINT('Ctrl Pts',(16.4060779675797,-0.174540169679895,
3.54017290856226));
#19193=CARTESIAN_POINT('Ctrl Pts',(16.4537938036425,0.292372898913969,3.60449612791703));
#19194=CARTESIAN_POINT('Ctrl Pts',(16.5015096397054,0.490795435699827,4.0320166386149));
#19195=CARTESIAN_POINT('Ctrl Pts',(16.5413781531317,0.280003220364278,4.36466130212541));
#19196=CARTESIAN_POINT('Ctrl Pts',(16.5653413878703,0.0704421061260754,
4.4151638399628));
#19197=CARTESIAN_POINT('Ctrl Pts',(16.5733993439214,-1.52272386678906E-5,
4.41518677123726));
#19198=CARTESIAN_POINT('Origin',(3.42660065607856,0.,4.));
#19199=CARTESIAN_POINT('',(15.8766006560786,-0.00023258108979477,4.41639972388928));
#19200=CARTESIAN_POINT('',(15.9733993439214,-0.000169011902647176,4.4164782780785));
#19201=CARTESIAN_POINT('',(3.42660065607856,4.87367679877478E-13,4.415875));
#19202=CARTESIAN_POINT('Ctrl Pts',(15.8766006560786,-0.000232581089794846,
4.41639972388928));
#19203=CARTESIAN_POINT('Ctrl Pts',(15.8781481639346,-0.0136633580705269,
4.41648966084242));
#19204=CARTESIAN_POINT('Ctrl Pts',(15.8956009504782,-0.165044849757219,
4.40979870506104));
#19205=CARTESIAN_POINT('Ctrl Pts',(15.9289590157095,-0.437567097060412,
4.22458909239344));
#19206=CARTESIAN_POINT('Ctrl Pts',(15.9766748517724,-0.425562075928853,
3.75341909160864));
#19207=CARTESIAN_POINT('Ctrl Pts',(16.0243906878352,-0.0227568523576073,
3.50868813313462));
#19208=CARTESIAN_POINT('Ctrl Pts',(16.072106523898,0.400946338892803,3.71513642180785));
#19209=CARTESIAN_POINT('Ctrl Pts',(16.1198223599609,0.456454337785543,4.1831793175245));
#19210=CARTESIAN_POINT('Ctrl Pts',(16.1546537373544,0.190990792023167,4.40204523666471));
#19211=CARTESIAN_POINT('Ctrl Pts',(16.1735798360603,0.0266382990664043,
4.41629648110721));
#19212=CARTESIAN_POINT('Ctrl Pts',(16.1766006560786,0.000364146841390366,
4.41605523138122));
#19213=CARTESIAN_POINT('Ctrl Pts',(15.9733993439214,-0.000169011902647174,
4.4164782780785));
#19214=CARTESIAN_POINT('Ctrl Pts',(15.974478043619,-0.00952634975615679,
4.4165263696097));
#19215=CARTESIAN_POINT('Ctrl Pts',(15.9914620220042,-0.156808910032117,
4.4119928338179));
#19216=CARTESIAN_POINT('Ctrl Pts',(16.024351279077,-0.430762722000766,4.23737881579128));
#19217=CARTESIAN_POINT('Ctrl Pts',(16.0720671151398,-0.432639725453012,
3.76605963834362));
#19218=CARTESIAN_POINT('Ctrl Pts',(16.1197829512026,-0.0372170120039125,
3.50957149464017));
#19219=CARTESIAN_POINT('Ctrl Pts',(16.1674987872655,0.392382656225717,3.70345139362117));
#19220=CARTESIAN_POINT('Ctrl Pts',(16.2152146233283,0.461651293660056,4.16965644082667));
#19221=CARTESIAN_POINT('Ctrl Pts',(16.2505148088803,0.199264245432362,4.39929555075695));
#19222=CARTESIAN_POINT('Ctrl Pts',(16.2699097157447,0.0307553622657438,
4.41621302761729));
#19223=CARTESIAN_POINT('Ctrl Pts',(16.2733993439214,0.000380345806842052,
4.41593091837313));
#19224=CARTESIAN_POINT('Origin',(3.42660065607856,0.,4.));
#19225=CARTESIAN_POINT('',(15.5766006560786,-0.000245472137683418,4.41533389801214));
#19226=CARTESIAN_POINT('',(15.6733993439214,-0.00029394562308721,4.41541483535501));
#19227=CARTESIAN_POINT('',(3.42660065607856,4.87367679877478E-13,4.415875));
#19228=CARTESIAN_POINT('Ctrl Pts',(15.5766006560786,-0.000245472137683396,
4.41533389801214));
#19229=CARTESIAN_POINT('Ctrl Pts',(15.5827164918089,-0.0536739331835165,
4.41562024719655));
#19230=CARTESIAN_POINT('Ctrl Pts',(15.6047376062269,-0.245697356182912,
4.38119912149661));
#19231=CARTESIAN_POINT('Ctrl Pts',(15.6426639993325,-0.483248643997369,
4.09152034160055));
#19232=CARTESIAN_POINT('Ctrl Pts',(15.6903798353953,-0.338341267922855,
3.64302603558196));
#19233=CARTESIAN_POINT('Ctrl Pts',(15.7380956714582,0.117270100534806,3.52234641383892));
#19234=CARTESIAN_POINT('Ctrl Pts',(15.785811507521,0.465190531238913,3.84030342991275));
#19235=CARTESIAN_POINT('Ctrl Pts',(15.8319798357278,0.388490242362186,4.28984418805176));
#19236=CARTESIAN_POINT('Ctrl Pts',(15.862242885247,0.124378106492246,4.41556528924811));
#19237=CARTESIAN_POINT('Ctrl Pts',(15.8766006560786,-0.000232581089794846,
4.41639972388928));
#19238=CARTESIAN_POINT('Ctrl Pts',(15.6733993439214,-0.000293945623087231,
4.41541483535501));
#19239=CARTESIAN_POINT('Ctrl Pts',(15.6790463714933,-0.0496027558454661,
4.41573527017753));
#19240=CARTESIAN_POINT('Ctrl Pts',(15.7005986777528,-0.23740431922453,4.38477730872224));
#19241=CARTESIAN_POINT('Ctrl Pts',(15.7380562626999,-0.480343569999647,
4.1057131950703));
#19242=CARTESIAN_POINT('Ctrl Pts',(15.7857720987628,-0.348708030819167,
3.6531456586776));
#19243=CARTESIAN_POINT('Ctrl Pts',(15.8334879348256,0.103151458625294,3.5190998009613));
#19244=CARTESIAN_POINT('Ctrl Pts',(15.8812037708885,0.460285376424935,3.82667199562295));
#19245=CARTESIAN_POINT('Ctrl Pts',(15.9278409072537,0.396214095655672,4.28286244744368));
#19246=CARTESIAN_POINT('Ctrl Pts',(15.9585727649314,0.128446309981357,4.41581726659612));
#19247=CARTESIAN_POINT('Ctrl Pts',(15.9733993439214,-0.000169011902647174,
4.4164782780785));
#19248=CARTESIAN_POINT('Origin',(3.42660065607856,0.,4.));
#19249=CARTESIAN_POINT('',(15.2766006560786,0.000330084823988869,4.41550084660604));
#19250=CARTESIAN_POINT('',(15.3733993439214,0.000289868078815952,4.41540680128743));
#19251=CARTESIAN_POINT('',(3.42660065607856,4.87367679877478E-13,4.415875));
#19252=CARTESIAN_POINT('Ctrl Pts',(15.2766006560786,0.000330084823988861,
4.41550084660604));
#19253=CARTESIAN_POINT('Ctrl Pts',(15.2872848196833,-0.0929135079625664,
4.41481081573461));
#19254=CARTESIAN_POINT('Ctrl Pts',(15.3138742619755,-0.32600240339937,4.33760928826424));
#19255=CARTESIAN_POINT('Ctrl Pts',(15.3563689829555,-0.489387968817152,
3.95096286275689));
#19256=CARTESIAN_POINT('Ctrl Pts',(15.4040848190183,-0.223435404337718,
3.56184267101825));
#19257=CARTESIAN_POINT('Ctrl Pts',(15.4518006550811,0.24770132994065,3.57508909640066));
#19258=CARTESIAN_POINT('Ctrl Pts',(15.499516491144,0.491370121559653,3.97853774265298));
#19259=CARTESIAN_POINT('Ctrl Pts',(15.5411164914764,0.310410063586636,4.3474585185963));
#19260=CARTESIAN_POINT('Ctrl Pts',(15.5668112131213,0.0852759340546689,
4.41487554708019));
#19261=CARTESIAN_POINT('Ctrl Pts',(15.5766006560786,-0.000245472137683396,
4.41533389801214));
#19262=CARTESIAN_POINT('Ctrl Pts',(15.3733993439214,0.000289868078815973,
4.41540680128743));
#19263=CARTESIAN_POINT('Ctrl Pts',(15.3836146993676,-0.0889130762729256,
4.41483587894927));
#19264=CARTESIAN_POINT('Ctrl Pts',(15.4097353335015,-0.317845114095608,
4.34285359523591));
#19265=CARTESIAN_POINT('Ctrl Pts',(15.4517612463229,-0.490619905976795,
3.96539750426199));
#19266=CARTESIAN_POINT('Ctrl Pts',(15.4994770823858,-0.236243011612202,
3.56861332390027));
#19267=CARTESIAN_POINT('Ctrl Pts',(15.5471929184486,0.235079475381852,3.56797816593814));
#19268=CARTESIAN_POINT('Ctrl Pts',(15.5949087545115,0.490524862970081,3.9640753057054));
#19269=CARTESIAN_POINT('Ctrl Pts',(15.6369775630024,0.318592711010818,4.34238143198936));
#19270=CARTESIAN_POINT('Ctrl Pts',(15.6631410928057,0.0892792238074376,
4.41483274135358));
#19271=CARTESIAN_POINT('Ctrl Pts',(15.6733993439214,-0.000293945623087231,
4.41541483535501));
#19272=CARTESIAN_POINT('Origin',(3.42660065607856,0.,4.));
#19273=CARTESIAN_POINT('',(14.9766006560786,0.000104941934236194,4.41652945172571));
#19274=CARTESIAN_POINT('',(15.0733993439214,0.000175165248676303,4.41647198785975));
#19275=CARTESIAN_POINT('',(3.42660065607856,4.87367679877478E-13,4.415875));
#19276=CARTESIAN_POINT('Ctrl Pts',(14.9766006560786,0.000104941934236227,
4.41652945172572));
#19277=CARTESIAN_POINT('Ctrl Pts',(14.9918531475576,-0.132161740438444,
4.41608294134065));
#19278=CARTESIAN_POINT('Ctrl Pts',(15.0230109177242,-0.40316752945992,4.27633971254324));
#19279=CARTESIAN_POINT('Ctrl Pts',(15.0700739665785,-0.455482716161518,
3.8144178884426));
#19280=CARTESIAN_POINT('Ctrl Pts',(15.1177898026413,-0.0902467530057116,
3.51651189422706));
#19281=CARTESIAN_POINT('Ctrl Pts',(15.1655056387041,0.357864192060027,3.66260046696357));
#19282=CARTESIAN_POINT('Ctrl Pts',(15.2132214747669,0.47734294310866,4.11852822244656));
#19283=CARTESIAN_POINT('Ctrl Pts',(15.2502531472251,0.229869832763757,4.3878938710325));
#19284=CARTESIAN_POINT('Ctrl Pts',(15.2713795409956,0.0458961718568525,
4.41583804947224));
#19285=CARTESIAN_POINT('Ctrl Pts',(15.2766006560786,0.000330084823988861,
4.41550084660604));
#19286=CARTESIAN_POINT('Ctrl Pts',(15.0733993439214,0.000175165248676341,
4.41647198785975));
#19287=CARTESIAN_POINT('Ctrl Pts',(15.0881830272419,-0.128073190246274,
4.41579247653651));
#19288=CARTESIAN_POINT('Ctrl Pts',(15.1188719892501,-0.395510344386944,
4.28350986851547));
#19289=CARTESIAN_POINT('Ctrl Pts',(15.1654662299459,-0.46075086019608,3.82791319143947));
#19290=CARTESIAN_POINT('Ctrl Pts',(15.2131820660087,-0.104447211543591,
3.51937956259357));
#19291=CARTESIAN_POINT('Ctrl Pts',(15.2608979020716,0.347771918596306,3.652207076714));
#19292=CARTESIAN_POINT('Ctrl Pts',(15.3086137381344,0.480626744730421,4.10441818376995));
#19293=CARTESIAN_POINT('Ctrl Pts',(15.346114218751,0.238163166260598,4.38445638366753));
#19294=CARTESIAN_POINT('Ctrl Pts',(15.36770942068,0.0499756483669043,4.41572480336754));
#19295=CARTESIAN_POINT('Ctrl Pts',(15.3733993439214,0.000289868078815973,
4.41540680128743));
#19296=CARTESIAN_POINT('Origin',(3.42660065607856,0.,4.));
#19297=CARTESIAN_POINT('',(14.6766006560786,-0.000383732061438463,4.41581798673635));
#19298=CARTESIAN_POINT('',(14.7733993439214,-0.000379407362125217,4.41594234696178));
#19299=CARTESIAN_POINT('',(3.42660065607856,4.87367679877478E-13,4.415875));
#19300=CARTESIAN_POINT('Ctrl Pts',(14.6766006560786,-0.000383732061438387,
4.41581798673635));
#19301=CARTESIAN_POINT('Ctrl Pts',(14.6805161967443,-0.0344897130604965,
4.41612948839573));
#19302=CARTESIAN_POINT('Ctrl Pts',(14.7003370160976,-0.206786574235377,
4.39667515056147));
#19303=CARTESIAN_POINT('Ctrl Pts',(14.7360631141386,-0.466025611307368,
4.15724297904063));
#19304=CARTESIAN_POINT('Ctrl Pts',(14.7837789502014,-0.38430721152129,3.69305832471834));
#19305=CARTESIAN_POINT('Ctrl Pts',(14.8314947862642,0.0503264139313189,
3.51074293371195));
#19306=CARTESIAN_POINT('Ctrl Pts',(14.8792106223271,0.438744519099385,3.77771983486548));
#19307=CARTESIAN_POINT('Ctrl Pts',(14.9269264583899,0.42425678142631,4.24882003188202));
#19308=CARTESIAN_POINT('Ctrl Pts',(14.9593898029737,0.149335702075518,4.41387566524124));
#19309=CARTESIAN_POINT('Ctrl Pts',(14.97594786887,0.00576578747519492,4.41654856180149));
#19310=CARTESIAN_POINT('Ctrl Pts',(14.9766006560786,0.000104941934236227,
4.41652945172572));
#19311=CARTESIAN_POINT('Ctrl Pts',(14.7733993439214,-0.000379407362125234,
4.41594234696178));
#19312=CARTESIAN_POINT('Ctrl Pts',(14.7768460764287,-0.0303789312965351,
4.41622104989506));
#19313=CARTESIAN_POINT('Ctrl Pts',(14.7961980876235,-0.198506931257387,
4.39955296987463));
#19314=CARTESIAN_POINT('Ctrl Pts',(14.831455377506,-0.461192356972643,4.17090007232882));
#19315=CARTESIAN_POINT('Ctrl Pts',(14.8791712135689,-0.393180492164677,
3.7045100248179));
#19316=CARTESIAN_POINT('Ctrl Pts',(14.9268870496317,0.0358950684576197,
3.50947296821438));
#19317=CARTESIAN_POINT('Ctrl Pts',(14.9746028856945,0.432007635398663,3.76489443262817));
#19318=CARTESIAN_POINT('Ctrl Pts',(15.0223187217574,0.431400943461215,4.23621695712364));
#19319=CARTESIAN_POINT('Ctrl Pts',(15.0552508744997,0.157562060208247,4.41179740605063));
#19320=CARTESIAN_POINT('Ctrl Pts',(15.0722777485543,0.00990499767517082,
4.41652354042182));
#19321=CARTESIAN_POINT('Ctrl Pts',(15.0733993439214,0.000175165248676341,
4.41647198785975));
#19322=CARTESIAN_POINT('Origin',(3.42660065607856,0.,4.));
#19323=CARTESIAN_POINT('',(14.3766006560786,7.63317591858645E-5,4.41519896243726));
#19324=CARTESIAN_POINT('',(14.4733993439214,9.02664646690309E-6,4.41518644689786));
#19325=CARTESIAN_POINT('',(3.42660065607856,4.87367679877478E-13,4.415875));
#19326=CARTESIAN_POINT('Ctrl Pts',(14.3766006560786,7.63317591858798E-5,
4.41519896243726));
#19327=CARTESIAN_POINT('Ctrl Pts',(14.3850845246186,-0.0740996743586071,
4.41507773880187));
#19328=CARTESIAN_POINT('Ctrl Pts',(14.4094736718463,-0.287504468978829,
4.360651101065));
#19329=CARTESIAN_POINT('Ctrl Pts',(14.4497680977616,-0.491476396904638,
4.01887262932433));
#19330=CARTESIAN_POINT('Ctrl Pts',(14.4974839338244,-0.281685449746218,
3.59681451879656));
#19331=CARTESIAN_POINT('Ctrl Pts',(14.5451997698872,0.186781580201919,3.54500783946397));
#19332=CARTESIAN_POINT('Ctrl Pts',(14.59291560595,0.483724211046603,3.91102746210588));
#19333=CARTESIAN_POINT('Ctrl Pts',(14.6367159013472,0.348540265561382,4.32201186060262));
#19334=CARTESIAN_POINT('Ctrl Pts',(14.6646109180567,0.104051852208848,4.41486414061182));
#19335=CARTESIAN_POINT('Ctrl Pts',(14.6766006560786,-0.000383732061438387,
4.41581798673635));
#19336=CARTESIAN_POINT('Ctrl Pts',(14.4733993439214,9.0266464668684E-6,
4.41518644689786));
#19337=CARTESIAN_POINT('Ctrl Pts',(14.481414404303,-0.0700733710850898,
4.41517292627706));
#19338=CARTESIAN_POINT('Ctrl Pts',(14.5053347433722,-0.279247125311621,
4.3650573561381));
#19339=CARTESIAN_POINT('Ctrl Pts',(14.545160361129,-0.490707361486496,4.03333931965322));
#19340=CARTESIAN_POINT('Ctrl Pts',(14.5928761971918,-0.293437803431633,
3.60528557111603));
#19341=CARTESIAN_POINT('Ctrl Pts',(14.6405920332547,0.173300204635467,3.53970415608515));
#19342=CARTESIAN_POINT('Ctrl Pts',(14.6883078693175,0.480893968219416,3.89681949708321));
#19343=CARTESIAN_POINT('Ctrl Pts',(14.7325769728731,0.356556173733762,4.31604662460621));
#19344=CARTESIAN_POINT('Ctrl Pts',(14.760940797741,0.10805675748006,4.41493494840171));
#19345=CARTESIAN_POINT('Ctrl Pts',(14.7733993439214,-0.000379407362125234,
4.41594234696178));
#19346=CARTESIAN_POINT('Origin',(3.42660065607856,0.,4.));
#19347=CARTESIAN_POINT('',(14.0766006560786,0.000355193352615291,4.41609897421413));
#19348=CARTESIAN_POINT('',(14.1733993439214,0.000376051973931104,4.41597558743442));
#19349=CARTESIAN_POINT('',(3.42660065607856,4.87367679877478E-13,4.415875));
#19350=CARTESIAN_POINT('Ctrl Pts',(14.0766006560786,0.000355193352615277,
4.41609897421413));
#19351=CARTESIAN_POINT('Ctrl Pts',(14.0896528524929,-0.113137957382804,
4.41506966208575));
#19352=CARTESIAN_POINT('Ctrl Pts',(14.1186103275949,-0.366637448157006,
4.30821039815648));
#19353=CARTESIAN_POINT('Ctrl Pts',(14.1634730813845,-0.476711717661702,
3.87895801102093));
#19354=CARTESIAN_POINT('Ctrl Pts',(14.2111889174473,-0.156014541823709,
3.53356170012368));
#19355=CARTESIAN_POINT('Ctrl Pts',(14.2589047535102,0.307953188363286,3.61650285707861));
#19356=CARTESIAN_POINT('Ctrl Pts',(14.306620589573,0.4891227672074,4.05161534124029));
#19357=CARTESIAN_POINT('Ctrl Pts',(14.3458525570958,0.268773633406098,4.37039329245586));
#19358=CARTESIAN_POINT('Ctrl Pts',(14.369179245931,0.0649630708582953,4.4153050049005));
#19359=CARTESIAN_POINT('Ctrl Pts',(14.3766006560786,7.63317591858798E-5,
4.41519896243726));
#19360=CARTESIAN_POINT('Ctrl Pts',(14.1733993439214,0.000376051973931098,
4.41597558743442));
#19361=CARTESIAN_POINT('Ctrl Pts',(14.1859827321773,-0.109124255432428,
4.41495896305428));
#19362=CARTESIAN_POINT('Ctrl Pts',(14.2144713991208,-0.358682910161539,
4.31442504752535));
#19363=CARTESIAN_POINT('Ctrl Pts',(14.258865344752,-0.480069828122688,3.8930505494253));
#19364=CARTESIAN_POINT('Ctrl Pts',(14.3065811808148,-0.169684322438749,
3.53835895376334));
#19365=CARTESIAN_POINT('Ctrl Pts',(14.3542970168777,0.296524907469595,3.60759943412104));
#19366=CARTESIAN_POINT('Ctrl Pts',(14.4020128529405,0.49043075222644,4.0371873919842));
#19367=CARTESIAN_POINT('Ctrl Pts',(14.4417136286217,0.277046036654804,4.36620192284859));
#19368=CARTESIAN_POINT('Ctrl Pts',(14.4655091256154,0.0689998253659925,
4.41519975692232));
#19369=CARTESIAN_POINT('Ctrl Pts',(14.4733993439214,9.0266464668684E-6,
4.41518644689786));
#19370=CARTESIAN_POINT('Origin',(3.42660065607856,0.,4.));
#19371=CARTESIAN_POINT('',(13.7766006560786,-0.000253139125078747,4.41636688691614));
#19372=CARTESIAN_POINT('',(13.8733993439214,-0.000192710833643805,4.4164526008213));
#19373=CARTESIAN_POINT('',(3.42660065607856,4.87367679877478E-13,4.415875));
#19374=CARTESIAN_POINT('Ctrl Pts',(13.7766006560786,-0.000253139125078718,
4.41636688691614));
#19375=CARTESIAN_POINT('Ctrl Pts',(13.7783159016796,-0.0151427949580853,
4.41647347977994));
#19376=CARTESIAN_POINT('Ctrl Pts',(13.7959364259683,-0.167994124135391,
4.40898222403799));
#19377=CARTESIAN_POINT('Ctrl Pts',(13.8294622289446,-0.439909757638992,
4.21996506537626));
#19378=CARTESIAN_POINT('Ctrl Pts',(13.8771780650075,-0.422939705734467,
3.74894775411238));
#19379=CARTESIAN_POINT('Ctrl Pts',(13.9248939010703,-0.0175776142901187,
3.50847558318244));
#19380=CARTESIAN_POINT('Ctrl Pts',(13.9726097371332,0.403926270823208,3.71937784729135));
#19381=CARTESIAN_POINT('Ctrl Pts',(14.020325573196,0.454498446235019,4.18797975215946));
#19382=CARTESIAN_POINT('Ctrl Pts',(14.0549892128445,0.188032430710383,4.40299531219535));
#19383=CARTESIAN_POINT('Ctrl Pts',(14.0737475738053,0.0251636842930195,
4.41632397176197));
#19384=CARTESIAN_POINT('Ctrl Pts',(14.0766006560786,0.000355193352615277,
4.41609897421413));
#19385=CARTESIAN_POINT('Ctrl Pts',(13.8733993439214,-0.000192710833643682,
4.4164526008213));
#19386=CARTESIAN_POINT('Ctrl Pts',(13.874645781364,-0.0110068809386406,
4.41651469495978));
#19387=CARTESIAN_POINT('Ctrl Pts',(13.8917974974943,-0.15975450351916,4.41122255187585));
#19388=CARTESIAN_POINT('Ctrl Pts',(13.9248544923121,-0.433240552373761,
4.23282579030437));
#19389=CARTESIAN_POINT('Ctrl Pts',(13.9725703283749,-0.430150181893835,
3.76151300691929));
#19390=CARTESIAN_POINT('Ctrl Pts',(14.0202861644378,-0.032046280669499,
3.50920649887429));
#19391=CARTESIAN_POINT('Ctrl Pts',(14.0680020005006,0.39548621318905,3.70760321474174));
#19392=CARTESIAN_POINT('Ctrl Pts',(14.1157178365634,0.459837632138507,4.1745123976147));
#19393=CARTESIAN_POINT('Ctrl Pts',(14.1508502843704,0.196303200904851,4.40029544879449));
#19394=CARTESIAN_POINT('Ctrl Pts',(14.1700774534897,0.0292830534939708,
4.41624396624722));
#19395=CARTESIAN_POINT('Ctrl Pts',(14.1733993439214,0.000376051973931098,
4.41597558743442));
#19396=CARTESIAN_POINT('Origin',(3.42660065607856,0.,4.));
#19397=CARTESIAN_POINT('',(13.4766006560786,-0.000226204729293368,4.4153088088013));
#19398=CARTESIAN_POINT('',(13.5733993439214,-0.000277574767750837,4.41538411867388));
#19399=CARTESIAN_POINT('',(3.42660065607856,4.87367679877478E-13,4.415875));
#19400=CARTESIAN_POINT('Ctrl Pts',(13.4766006560786,-0.000226204729293314,
4.4153088088013));
#19401=CARTESIAN_POINT('Ctrl Pts',(13.482884229554,-0.0551283395969922,
4.41557894444213));
#19402=CARTESIAN_POINT('Ctrl Pts',(13.505073081717,-0.248664136397309,4.37988069596112));
#19403=CARTESIAN_POINT('Ctrl Pts',(13.5431672125676,-0.484186345555107,
4.08642226350871));
#19404=CARTESIAN_POINT('Ctrl Pts',(13.5908830486304,-0.334560300710407,
3.63948005597396));
#19405=CARTESIAN_POINT('Ctrl Pts',(13.6385988846933,0.122297616148583,3.52360886035071));
#19406=CARTESIAN_POINT('Ctrl Pts',(13.6863147207561,0.466847750307624,3.8452149784873));
#19407=CARTESIAN_POINT('Ctrl Pts',(13.7323153112179,0.38570983934117,4.29229218593957));
#19408=CARTESIAN_POINT('Ctrl Pts',(13.762410622992,0.122927301498021,4.41548505619568));
#19409=CARTESIAN_POINT('Ctrl Pts',(13.7766006560786,-0.000253139125078718,
4.41636688691614));
#19410=CARTESIAN_POINT('Ctrl Pts',(13.5733993439214,-0.000277574767750817,
4.41538411867388));
#19411=CARTESIAN_POINT('Ctrl Pts',(13.5792141092383,-0.0510604653080308,
4.41569425641003));
#19412=CARTESIAN_POINT('Ctrl Pts',(13.6009341532429,-0.240371663949131,
4.38351498152559));
#19413=CARTESIAN_POINT('Ctrl Pts',(13.6385594759351,-0.481431012491488,
4.10064494554323));
#19414=CARTESIAN_POINT('Ctrl Pts',(13.6862753119979,-0.345033139360895,
3.64948986092447));
#19415=CARTESIAN_POINT('Ctrl Pts',(13.7339911480608,0.108213974662067,3.52021363031051));
#19416=CARTESIAN_POINT('Ctrl Pts',(13.7817069841236,0.462086530666827,3.83153260544464));
#19417=CARTESIAN_POINT('Ctrl Pts',(13.8281763827438,0.393458703070077,4.28538422885222));
#19418=CARTESIAN_POINT('Ctrl Pts',(13.8587405026764,0.126988323162951,4.4157223370415));
#19419=CARTESIAN_POINT('Ctrl Pts',(13.8733993439214,-0.000192710833643682,
4.4164526008213));
#19420=CARTESIAN_POINT('Origin',(3.42660065607856,0.,4.));
#19421=CARTESIAN_POINT('',(13.1766006560786,0.000342007958933446,4.41553758638116));
#19422=CARTESIAN_POINT('',(13.2733993439214,0.000305371599794934,4.41543889539504));
#19423=CARTESIAN_POINT('',(3.42660065607856,4.87367679877478E-13,4.415875));
#19424=CARTESIAN_POINT('Ctrl Pts',(13.1766006560786,0.000342007958933428,
4.41553758638117));
#19425=CARTESIAN_POINT('Ctrl Pts',(13.1874525574283,-0.0943443719380771,
4.41480703635833));
#19426=CARTESIAN_POINT('Ctrl Pts',(13.2142097374657,-0.328913583769224,
4.33568767983454));
#19427=CARTESIAN_POINT('Ctrl Pts',(13.2568721961906,-0.488843983144383,
3.94580788806928));
#19428=CARTESIAN_POINT('Ctrl Pts',(13.3045880322534,-0.218805220893238,
3.55951220202843));
#19429=CARTESIAN_POINT('Ctrl Pts',(13.3523038683163,0.252165742455243,3.57772323864086));
#19430=CARTESIAN_POINT('Ctrl Pts',(13.4000197043791,0.491569024438394,3.98371752277252));
#19431=CARTESIAN_POINT('Ctrl Pts',(13.4414519669665,0.307476227900318,4.34923088347422));
#19432=CARTESIAN_POINT('Ctrl Pts',(13.4669789508664,0.0838425436168888,
4.41489516431802));
#19433=CARTESIAN_POINT('Ctrl Pts',(13.4766006560786,-0.000226204729293314,
4.4153088088013));
#19434=CARTESIAN_POINT('Ctrl Pts',(13.2733993439214,0.000305371599794949,
4.41543889539504));
#19435=CARTESIAN_POINT('Ctrl Pts',(13.2837824371127,-0.0903447040275099,
4.41482455235666));
#19436=CARTESIAN_POINT('Ctrl Pts',(13.3100708089916,-0.320767143545349,
4.3409984814332));
#19437=CARTESIAN_POINT('Ctrl Pts',(13.352264459558,-0.490227979701372,3.96022874442655));
#19438=CARTESIAN_POINT('Ctrl Pts',(13.3999802956209,-0.23168347330409,3.56614749850931));
#19439=CARTESIAN_POINT('Ctrl Pts',(13.4476961316837,0.239619531536799,3.57047968038978));
#19440=CARTESIAN_POINT('Ctrl Pts',(13.4954119677466,0.490876233547033,3.96924698078795));
#19441=CARTESIAN_POINT('Ctrl Pts',(13.5373130384925,0.315668023336251,4.34421900798688));
#19442=CARTESIAN_POINT('Ctrl Pts',(13.5633088305507,0.0878472949503496,
4.41484592860038));
#19443=CARTESIAN_POINT('Ctrl Pts',(13.5733993439214,-0.000277574767750817,
4.41538411867388));
#19444=CARTESIAN_POINT('Origin',(3.42660065607856,0.,4.));
#19445=CARTESIAN_POINT('',(12.8766006560786,7.85109994957766E-5,4.41654344863055));
#19446=CARTESIAN_POINT('',(12.9733993439214,0.000150764780949702,4.41649545414489));
#19447=CARTESIAN_POINT('',(3.42660065607856,4.87367679877478E-13,4.415875));
#19448=CARTESIAN_POINT('Ctrl Pts',(12.8766006560786,7.85109994958138E-5,
4.41654344863055));
#19449=CARTESIAN_POINT('Ctrl Pts',(12.8920208853026,-0.133630732206743,
4.41619751255639));
#19450=CARTESIAN_POINT('Ctrl Pts',(12.9233463932143,-0.405888408666218,
4.27372356364211));
#19451=CARTESIAN_POINT('Ctrl Pts',(12.9705771798136,-0.453501555338242,
3.80962782724943));
#19452=CARTESIAN_POINT('Ctrl Pts',(13.0182930158764,-0.0851462219395619,
3.51558762841831));
#19453=CARTESIAN_POINT('Ctrl Pts',(13.0660088519392,0.361400197209248,3.66639076405307));
#19454=CARTESIAN_POINT('Ctrl Pts',(13.1137246880021,0.476067254403989,4.1235523942958));
#19455=CARTESIAN_POINT('Ctrl Pts',(13.1505886227152,0.226902767145371,4.38908671404106));
#19456=CARTESIAN_POINT('Ctrl Pts',(13.1715472787407,0.0444343739838573,
4.41587777975472));
#19457=CARTESIAN_POINT('Ctrl Pts',(13.1766006560786,0.000342007958933428,
4.41553758638117));
#19458=CARTESIAN_POINT('Ctrl Pts',(12.9733993439214,0.000150764780949724,
4.4164954541449));
#19459=CARTESIAN_POINT('Ctrl Pts',(12.988350764987,-0.12953330947047,4.41589144324702));
#19460=CARTESIAN_POINT('Ctrl Pts',(13.0192074647402,-0.39825874617628,4.28096832590395));
#19461=CARTESIAN_POINT('Ctrl Pts',(13.065969443181,-0.458911634846768,3.82306685936703));
#19462=CARTESIAN_POINT('Ctrl Pts',(13.1136852792439,-0.0993761143989603,
3.51830547777773));
#19463=CARTESIAN_POINT('Ctrl Pts',(13.1614011153067,0.351418020999476,3.65589158776806));
#19464=CARTESIAN_POINT('Ctrl Pts',(13.2091169513695,0.479499580452807,4.10947774749948));
#19465=CARTESIAN_POINT('Ctrl Pts',(13.2464496942411,0.235195791588524,4.38570395495548));
#19466=CARTESIAN_POINT('Ctrl Pts',(13.2678771584251,0.0485170676377186,
4.41576563003508));
#19467=CARTESIAN_POINT('Ctrl Pts',(13.2733993439214,0.000305371599794949,
4.41543889539504));
#19468=CARTESIAN_POINT('Origin',(3.42660065607856,0.,4.));
#19469=CARTESIAN_POINT('',(12.5766006560786,-0.000382134531266273,4.41577416496379));
#19470=CARTESIAN_POINT('',(12.6733993439214,-0.000382453243898073,4.41589767499446));
#19471=CARTESIAN_POINT('',(3.42660065607856,4.87367679877478E-13,4.415875));
#19472=CARTESIAN_POINT('Ctrl Pts',(12.5766006560786,-0.000382134531266193,
4.41577416496379));
#19473=CARTESIAN_POINT('Ctrl Pts',(12.5806839344893,-0.0359587315295452,
4.41609477791077));
#19474=CARTESIAN_POINT('Ctrl Pts',(12.6006724915877,-0.209750441210566,
4.39561070447123));
#19475=CARTESIAN_POINT('Ctrl Pts',(12.6365663273737,-0.4676569254097,4.15232276575852));
#19476=CARTESIAN_POINT('Ctrl Pts',(12.6842821634365,-0.381050985679211,
3.68902512775968));
#19477=CARTESIAN_POINT('Ctrl Pts',(12.7319979994994,0.0554799374235607,
3.5113004999026));
#19478=CARTESIAN_POINT('Ctrl Pts',(12.7797138355622,0.441062780321708,3.78235614259331));
#19479=CARTESIAN_POINT('Ctrl Pts',(12.8274296716251,0.421610885427219,4.2532774884218));
#19480=CARTESIAN_POINT('Ctrl Pts',(12.8597252784638,0.146394963767536,4.4145887178469));
#19481=CARTESIAN_POINT('Ctrl Pts',(12.876115606615,0.00428438860018927,
4.4165543301878));
#19482=CARTESIAN_POINT('Ctrl Pts',(12.8766006560786,7.85109994958138E-5,
4.41654344863055));
#19483=CARTESIAN_POINT('Ctrl Pts',(12.6733993439214,-0.000382453243898042,
4.41589767499447));
#19484=CARTESIAN_POINT('Ctrl Pts',(12.6770138141737,-0.0318505807336982,
4.4161892599907));
#19485=CARTESIAN_POINT('Ctrl Pts',(12.6965335631136,-0.201468625965512,
4.39853963407534));
#19486=CARTESIAN_POINT('Ctrl Pts',(12.7319585907412,-0.462967872677167,
4.16603003860975));
#19487=CARTESIAN_POINT('Ctrl Pts',(12.779674426804,-0.390044463885,3.70038267566003));
#19488=CARTESIAN_POINT('Ctrl Pts',(12.8273902628668,0.0410627776982723,
3.50987851185683));
#19489=CARTESIAN_POINT('Ctrl Pts',(12.8751060989297,0.434461438689172,3.76946045210395));
#19490=CARTESIAN_POINT('Ctrl Pts',(12.9228219349925,0.42888747548329,4.24075040649094));
#19491=CARTESIAN_POINT('Ctrl Pts',(12.9555863499897,0.154617472482897,4.41255553662561));
#19492=CARTESIAN_POINT('Ctrl Pts',(12.9724454862994,0.00842423538524961,
4.41653398830136));
#19493=CARTESIAN_POINT('Ctrl Pts',(12.9733993439214,0.000150764780949724,
4.4164954541449));
#19494=CARTESIAN_POINT('Origin',(3.42660065607856,0.,4.));
#19495=CARTESIAN_POINT('',(12.2766006560786,9.99581421417901E-5,4.41520820259509));
#19496=CARTESIAN_POINT('',(12.3733993439214,3.32456539758885E-5,4.41518865831861));
#19497=CARTESIAN_POINT('',(3.42660065607856,4.87367679877478E-13,4.415875));
#19498=CARTESIAN_POINT('Ctrl Pts',(12.2766006560786,9.99581421418094E-5,
4.41520820259509));
#19499=CARTESIAN_POINT('Ctrl Pts',(12.2852522623637,-0.0755384113923865,
4.41504611816934));
#19500=CARTESIAN_POINT('Ctrl Pts',(12.3098091473364,-0.290455378639464,
4.35903266527152));
#19501=CARTESIAN_POINT('Ctrl Pts',(12.3502713109967,-0.49164800158875,4.0136918729824));
#19502=CARTESIAN_POINT('Ctrl Pts',(12.3979871470595,-0.277420602272412,
3.59386820576715));
#19503=CARTESIAN_POINT('Ctrl Pts',(12.4457029831224,0.191566404775332,3.54700161433684));
#19504=CARTESIAN_POINT('Ctrl Pts',(12.4934188191852,0.484635034689867,3.91613041073711));
#19505=CARTESIAN_POINT('Ctrl Pts',(12.5370513768373,0.345661459897227,4.32409890635003));
#19506=CARTESIAN_POINT('Ctrl Pts',(12.5647786558017,0.102620036091023,4.41484591908716));
#19507=CARTESIAN_POINT('Ctrl Pts',(12.5766006560786,-0.000382134531266193,
4.41577416496379));
#19508=CARTESIAN_POINT('Ctrl Pts',(12.3733993439214,3.32456539758746E-5,
4.41518865831861));
#19509=CARTESIAN_POINT('Ctrl Pts',(12.381582142048,-0.071514873974996,4.41513780400291));
#19510=CARTESIAN_POINT('Ctrl Pts',(12.4056702188623,-0.282203129244181,
4.36350051499509));
#19511=CARTESIAN_POINT('Ctrl Pts',(12.4456635743641,-0.491031474462283,
4.0281658647901));
#19512=CARTESIAN_POINT('Ctrl Pts',(12.493379410427,-0.289261580343189,3.60221492864948));
#19513=CARTESIAN_POINT('Ctrl Pts',(12.5410952464898,0.178141673866572,3.54155614424011));
#19514=CARTESIAN_POINT('Ctrl Pts',(12.5888110825527,0.481954687902679,3.90189340664049));
#19515=CARTESIAN_POINT('Ctrl Pts',(12.6329124483632,0.353693368040787,4.31820342736526));
#19516=CARTESIAN_POINT('Ctrl Pts',(12.6611085354861,0.106623193447456,4.41490615616012));
#19517=CARTESIAN_POINT('Ctrl Pts',(12.6733993439214,-0.000382453243898042,
4.41589767499447));
#19518=CARTESIAN_POINT('Origin',(3.42660065607856,0.,4.));
#19519=CARTESIAN_POINT('',(11.9766006560786,0.000344603143201134,4.41614202049347));
#19520=CARTESIAN_POINT('',(12.0733993439214,0.00037008249145147,4.41602009379307));
#19521=CARTESIAN_POINT('',(3.42660065607856,4.87367679877478E-13,4.415875));
#19522=CARTESIAN_POINT('Ctrl Pts',(11.9766006560786,0.000344603143201134,
4.41614202049347));
#19523=CARTESIAN_POINT('Ctrl Pts',(11.989820590238,-0.114576335025177,4.41511745277426));
#19524=CARTESIAN_POINT('Ctrl Pts',(12.018945803085,-0.369470719226983,4.30593844396252));
#19525=CARTESIAN_POINT('Ctrl Pts',(12.0639762946196,-0.475409571231627,
3.87394063131468));
#19526=CARTESIAN_POINT('Ctrl Pts',(12.1116921306825,-0.151090047408964,
3.53194335553704));
#19527=CARTESIAN_POINT('Ctrl Pts',(12.1594079667453,0.311977791768556,3.61976969834691));
#19528=CARTESIAN_POINT('Ctrl Pts',(12.2071238028081,0.488551624369653,4.05676737776005));
#19529=CARTESIAN_POINT('Ctrl Pts',(12.2461880325859,0.265811525316043,4.37185240566124));
#19530=CARTESIAN_POINT('Ctrl Pts',(12.269346983676,0.0635166157645696,4.41534409728183));
#19531=CARTESIAN_POINT('Ctrl Pts',(12.2766006560786,9.99581421418094E-5,
4.41520820259509));
#19532=CARTESIAN_POINT('Ctrl Pts',(12.0733993439214,0.000370082491451453,
4.41602009379308));
#19533=CARTESIAN_POINT('Ctrl Pts',(12.0861504699224,-0.110559366248508,
4.41499479059613));
#19534=CARTESIAN_POINT('Ctrl Pts',(12.1148068746109,-0.361534897467509,
4.3122242613332));
#19535=CARTESIAN_POINT('Ctrl Pts',(12.1593685579871,-0.478916017555994,
3.88799699566402));
#19536=CARTESIAN_POINT('Ctrl Pts',(12.2070843940499,-0.164809627468288,
3.53659627586117));
#19537=CARTESIAN_POINT('Ctrl Pts',(12.2548002301128,0.300643979445627,3.61074632631782));
#19538=CARTESIAN_POINT('Ctrl Pts',(12.3025160661756,0.490011594032383,4.04235401475446));
#19539=CARTESIAN_POINT('Ctrl Pts',(12.3420491041118,0.274087380788525,4.36772087084377));
#19540=CARTESIAN_POINT('Ctrl Pts',(12.3656768633604,0.0675564760281007,
4.41523665186048));
#19541=CARTESIAN_POINT('Ctrl Pts',(12.3733993439214,3.32456539758746E-5,
4.41518865831861));
#19542=CARTESIAN_POINT('Origin',(3.42660065607856,0.,4.));
#19543=CARTESIAN_POINT('',(11.6766006560786,-0.000272404999166542,4.41633191892761));
#19544=CARTESIAN_POINT('',(11.7733993439214,-0.000215373091504267,4.41642415578018));
#19545=CARTESIAN_POINT('',(3.42660065607856,4.87367679877478E-13,4.415875));
#19546=CARTESIAN_POINT('Ctrl Pts',(11.6766006560786,-0.000272404999166455,
4.41633191892761));
#19547=CARTESIAN_POINT('Ctrl Pts',(11.6784836394247,-0.0166217551361539,
4.41645573239506));
#19548=CARTESIAN_POINT('Ctrl Pts',(11.6962719014584,-0.170944672110958,
4.40814899119985));
#19549=CARTESIAN_POINT('Ctrl Pts',(11.7299654421798,-0.44220355512924,4.21531660568344));
#19550=CARTESIAN_POINT('Ctrl Pts',(11.7776812782426,-0.420270357404582,
3.74450430230823));
#19551=CARTESIAN_POINT('Ctrl Pts',(11.8253971143054,-0.0123964237846327,
3.50831762943));
#19552=CARTESIAN_POINT('Ctrl Pts',(11.8731129503683,0.406861336540243,3.72365044295193));
#19553=CARTESIAN_POINT('Ctrl Pts',(11.9208287864311,0.452492071153857,4.1927593068956));
#19554=CARTESIAN_POINT('Ctrl Pts',(11.9553246883346,0.185075114683736,4.40392780377));
#19555=CARTESIAN_POINT('Ctrl Pts',(11.9739153115504,0.0236883133891,4.41635013933017));
#19556=CARTESIAN_POINT('Ctrl Pts',(11.9766006560786,0.000344603143201134,
4.41614202049347));
#19557=CARTESIAN_POINT('Ctrl Pts',(11.7733993439214,-0.000215373091504231,
4.41642415578018));
#19558=CARTESIAN_POINT('Ctrl Pts',(11.7748135191091,-0.0124870613922979,
4.41650138834433));
#19559=CARTESIAN_POINT('Ctrl Pts',(11.7921329729843,-0.162701432614141,
4.41043584391465));
#19560=CARTESIAN_POINT('Ctrl Pts',(11.8253577055472,-0.435670260442099,
4.22824690363353));
#19561=CARTESIAN_POINT('Ctrl Pts',(11.8730735416101,-0.427612859293677,
3.75699286549843));
#19562=CARTESIAN_POINT('Ctrl Pts',(11.9207893776729,-0.0268719897862959,
3.50889601812151));
#19563=CARTESIAN_POINT('Ctrl Pts',(11.9685052137357,0.398545841420554,3.71178751390968));
#19564=CARTESIAN_POINT('Ctrl Pts',(12.0162210497986,0.457972894034889,4.17934897039372));
#19565=CARTESIAN_POINT('Ctrl Pts',(12.0511857598605,0.193343073938706,4.40127740506484));
#19566=CARTESIAN_POINT('Ctrl Pts',(12.0702451912347,0.0278098881012828,
4.41627371553856));
#19567=CARTESIAN_POINT('Ctrl Pts',(12.0733993439214,0.000370082491451453,
4.41602009379308));
#19568=CARTESIAN_POINT('Origin',(3.42660065607856,0.,4.));
#19569=CARTESIAN_POINT('',(11.3766006560786,-0.000206048103233091,4.41528588740701));
#19570=CARTESIAN_POINT('',(11.4733993439214,-0.000260100423148973,4.41535533657191));
#19571=CARTESIAN_POINT('',(3.42660065607856,4.87367679877478E-13,4.415875));
#19572=CARTESIAN_POINT('Ctrl Pts',(11.3766006560786,-0.000206048103232999,
4.41528588740701));
#19573=CARTESIAN_POINT('Ctrl Pts',(11.383051967299,-0.0565815589273492,
4.41553770218085));
#19574=CARTESIAN_POINT('Ctrl Pts',(11.4054085572071,-0.251630532720247,
4.37854193442951));
#19575=CARTESIAN_POINT('Ctrl Pts',(11.4436704258028,-0.485070265991237,
4.08131458604192));
#19576=CARTESIAN_POINT('Ctrl Pts',(11.4913862618656,-0.330742172127369,
3.63597412121053));
#19577=CARTESIAN_POINT('Ctrl Pts',(11.5391020979284,0.127311547523522,3.52492422212962));
#19578=CARTESIAN_POINT('Ctrl Pts',(11.5868179339912,0.468453114143607,3.85014371984754));
#19579=CARTESIAN_POINT('Ctrl Pts',(11.632650786708,0.382920955827079,4.29471395365306));
#19580=CARTESIAN_POINT('Ctrl Pts',(11.6625783607371,0.121478760105588,4.41540989855421));
#19581=CARTESIAN_POINT('Ctrl Pts',(11.6766006560786,-0.000272404999166455,
4.41633191892761));
#19582=CARTESIAN_POINT('Ctrl Pts',(11.4733993439214,-0.000260100423148869,
4.41535533657191));
#19583=CARTESIAN_POINT('Ctrl Pts',(11.4793818469834,-0.0525169974224216,
4.41565306322741));
#19584=CARTESIAN_POINT('Ctrl Pts',(11.501269628733,-0.243338890257842,4.3822327073369));
#19585=CARTESIAN_POINT('Ctrl Pts',(11.5390626891702,-0.482464979911041,
4.09556551685319));
#19586=CARTESIAN_POINT('Ctrl Pts',(11.586778525233,-0.341319923258817,3.64587299617429));
#19587=CARTESIAN_POINT('Ctrl Pts',(11.6344943612959,0.113264470804062,3.5213807520529));
#19588=CARTESIAN_POINT('Ctrl Pts',(11.6822101973587,0.463836358529674,3.83641192782507));
#19589=CARTESIAN_POINT('Ctrl Pts',(11.7285118582339,0.390694138047139,4.28787953265104));
#19590=CARTESIAN_POINT('Ctrl Pts',(11.7589082404215,0.125533053862222,4.41563275094549));
#19591=CARTESIAN_POINT('Ctrl Pts',(11.7733993439214,-0.000215373091504231,
4.41642415578018));
#19592=CARTESIAN_POINT('Origin',(3.42660065607856,0.,4.));
#19593=CARTESIAN_POINT('',(11.0766006560786,0.000352537510456688,4.41557576695298));
#19594=CARTESIAN_POINT('',(11.1733993439214,0.000319650745578964,4.41547275084625));
#19595=CARTESIAN_POINT('',(3.42660065607856,4.87367679877478E-13,4.415875));
#19596=CARTESIAN_POINT('Ctrl Pts',(11.0766006560786,0.000352537510456667,
4.41557576695298));
#19597=CARTESIAN_POINT('Ctrl Pts',(11.0876202951733,-0.0957751134661499,
4.41480617263661));
#19598=CARTESIAN_POINT('Ctrl Pts',(11.1145452129557,-0.331820540820521,
4.33374203885914));
#19599=CARTESIAN_POINT('Ctrl Pts',(11.1573754094257,-0.488245699001722,
3.94065893278431));
#19600=CARTESIAN_POINT('Ctrl Pts',(11.2050912454886,-0.214150733603143,
3.55723066033293));
#19601=CARTESIAN_POINT('Ctrl Pts',(11.2528070815514,0.256602145595791,3.58040428537983));
#19602=CARTESIAN_POINT('Ctrl Pts',(11.3005229176142,0.491713326162588,3.98889911147238));
#19603=CARTESIAN_POINT('Ctrl Pts',(11.3417874424566,0.304539430122629,4.35098016691413));
#19604=CARTESIAN_POINT('Ctrl Pts',(11.3671466886114,0.0824085130402235,
4.41491686960609));
#19605=CARTESIAN_POINT('Ctrl Pts',(11.3766006560786,-0.000206048103232999,
4.41528588740701));
#19606=CARTESIAN_POINT('Ctrl Pts',(11.1733993439214,0.000319650745578978,
4.41547275084625));
#19607=CARTESIAN_POINT('Ctrl Pts',(11.1839501748577,-0.0917759901056567,
4.4148158243975));
#19608=CARTESIAN_POINT('Ctrl Pts',(11.2104062844816,-0.32368545017211,4.33911969104981));
#19609=CARTESIAN_POINT('Ctrl Pts',(11.2527676727932,-0.489781601228288,
3.95506440219344));
#19610=CARTESIAN_POINT('Ctrl Pts',(11.300483508856,-0.227098200695192,3.56372986339542));
#19611=CARTESIAN_POINT('Ctrl Pts',(11.3481993449188,0.244132971891272,3.57302890392028));
#19612=CARTESIAN_POINT('Ctrl Pts',(11.3959151809817,0.491173079921361,3.97442207176994));
#19613=CARTESIAN_POINT('Ctrl Pts',(11.4376485139825,0.312739912806573,4.34603313379779));
#19614=CARTESIAN_POINT('Ctrl Pts',(11.4634765682958,0.0864149014017155,
4.41486151738456));
#19615=CARTESIAN_POINT('Ctrl Pts',(11.4733993439214,-0.000260100423148869,
4.41535533657191));
#19616=CARTESIAN_POINT('Origin',(3.42660065607856,0.,4.));
#19617=CARTESIAN_POINT('',(10.7766006560786,5.16128798610187E-5,4.41655360457584));
#19618=CARTESIAN_POINT('',(10.8733993439214,0.000125523266313186,4.41651574507477));
#19619=CARTESIAN_POINT('',(3.42660065607856,4.87367679877478E-13,4.415875));
#19620=CARTESIAN_POINT('Ctrl Pts',(10.7766006560786,5.16128798610299E-5,
4.41655360457584));
#19621=CARTESIAN_POINT('Ctrl Pts',(10.7921886230477,-0.135103241057852,
4.41631783152902));
#19622=CARTESIAN_POINT('Ctrl Pts',(10.8236818687044,-0.408598944994929,
4.27108057505162));
#19623=CARTESIAN_POINT('Ctrl Pts',(10.8710803930487,-0.451470021714238,
3.80485891169382));
#19624=CARTESIAN_POINT('Ctrl Pts',(10.9187962291115,-0.080036233235122,
3.51471716883706));
#19625=CARTESIAN_POINT('Ctrl Pts',(10.9665120651743,0.364896059739551,3.6702181168734));
#19626=CARTESIAN_POINT('Ctrl Pts',(11.0142279012372,0.47473868640782,4.1285628425314));
#19627=CARTESIAN_POINT('Ctrl Pts',(11.0509240982053,0.223935965514619,4.3902602363912));
#19628=CARTESIAN_POINT('Ctrl Pts',(11.0717150164857,0.0429714521173939,
4.4159169723618));
#19629=CARTESIAN_POINT('Ctrl Pts',(11.0766006560786,0.000352537510456667,
4.41557576695298));
#19630=CARTESIAN_POINT('Ctrl Pts',(10.8733993439214,0.000125523266313226,
4.41651574507477));
#19631=CARTESIAN_POINT('Ctrl Pts',(10.888518502732,-0.130996444363694,4.41599591363288));
#19632=CARTESIAN_POINT('Ctrl Pts',(10.9195429402303,-0.400997532511054,
4.27840016053723));
#19633=CARTESIAN_POINT('Ctrl Pts',(10.9664726564161,-0.45702143577077,3.81824018018824));
#19634=CARTESIAN_POINT('Ctrl Pts',(11.014188492479,-0.0942939790271268,
3.51728489730359));
#19635=CARTESIAN_POINT('Ctrl Pts',(11.0619043285418,0.355025089556487,3.65961432075161));
#19636=CARTESIAN_POINT('Ctrl Pts',(11.1096201646047,0.478319155637209,4.11452515096033));
#19637=CARTESIAN_POINT('Ctrl Pts',(11.1467851697312,0.23222845252417,4.38693182090163));
#19638=CARTESIAN_POINT('Ctrl Pts',(11.1680448961701,0.0470573247768451,
4.41580613485813));
#19639=CARTESIAN_POINT('Ctrl Pts',(11.1733993439214,0.000319650745578978,
4.41547275084625));
#19640=CARTESIAN_POINT('Origin',(3.42660065607856,0.,4.));
#19641=CARTESIAN_POINT('',(10.4766006560786,-0.000378910032885682,4.4157309619862));
#19642=CARTESIAN_POINT('',(10.5733993439214,-0.000383826598418624,4.41585315377736));
#19643=CARTESIAN_POINT('',(3.42660065607856,4.87367679877478E-13,4.415875));
#19644=CARTESIAN_POINT('Ctrl Pts',(10.4766006560786,-0.000378910032885704,
4.4157309619862));
#19645=CARTESIAN_POINT('Ctrl Pts',(10.4808516722344,-0.0374267536145521,
4.41605913507464));
#19646=CARTESIAN_POINT('Ctrl Pts',(10.5010079670778,-0.212714974368116,
4.3945277200383));
#19647=CARTESIAN_POINT('Ctrl Pts',(10.5370695406088,-0.469236294399976,
4.14738563318641));
#19648=CARTESIAN_POINT('Ctrl Pts',(10.5847853766716,-0.377752434501872,
3.68502647241413));
#19649=CARTESIAN_POINT('Ctrl Pts',(10.6325012127345,0.0606272984676223,
3.51191234851464));
#19650=CARTESIAN_POINT('Ctrl Pts',(10.6802170487973,0.443332050383407,3.78701662516801));
#19651=CARTESIAN_POINT('Ctrl Pts',(10.7279328848602,0.418918158891686,4.25770681210006));
#19652=CARTESIAN_POINT('Ctrl Pts',(10.7600607539539,0.143455624352724,4.41528584951654));
#19653=CARTESIAN_POINT('Ctrl Pts',(10.7762833443601,0.00280285164340033,
4.41655840401831));
#19654=CARTESIAN_POINT('Ctrl Pts',(10.7766006560786,5.16128798610299E-5,
4.41655360457584));
#19655=CARTESIAN_POINT('Ctrl Pts',(10.5733993439214,-0.000383826598418617,
4.41585315377736));
#19656=CARTESIAN_POINT('Ctrl Pts',(10.5771815519187,-0.0333213161677604,
4.41615637378185));
#19657=CARTESIAN_POINT('Ctrl Pts',(10.5968690386037,-0.20443114816448,4.39750812937281));
#19658=CARTESIAN_POINT('Ctrl Pts',(10.6324618039763,-0.464691964107356,
4.16114156306187));
#19659=CARTESIAN_POINT('Ctrl Pts',(10.6801776400391,-0.386865111317189,
3.69628860657276));
#19660=CARTESIAN_POINT('Ctrl Pts',(10.7278934761019,0.0462259258804368,
3.51033849586834));
#19661=CARTESIAN_POINT('Ctrl Pts',(10.7756093121648,0.436866984064762,3.77405207881873));
#19662=CARTESIAN_POINT('Ctrl Pts',(10.8233251482276,0.426326368719826,4.24525711444552));
#19663=CARTESIAN_POINT('Ctrl Pts',(10.8559218254798,0.151674250044741,4.4132974389186));
#19664=CARTESIAN_POINT('Ctrl Pts',(10.8726132240444,0.00694320316194716,
4.41654277368359));
#19665=CARTESIAN_POINT('Ctrl Pts',(10.8733993439214,0.000125523266313226,
4.41651574507477));
#19666=CARTESIAN_POINT('Origin',(3.42660065607856,0.,4.));
#19667=CARTESIAN_POINT('',(10.1766006560786,0.000123197149224082,4.41521991402453));
#19668=CARTESIAN_POINT('',(10.2733993439214,5.7336166378985E-5,4.41519339896199));
#19669=CARTESIAN_POINT('',(3.42660065607856,4.87367679877478E-13,4.415875));
#19670=CARTESIAN_POINT('Ctrl Pts',(10.1766006560786,0.000123197149224097,
4.41521991402453));
#19671=CARTESIAN_POINT('Ctrl Pts',(10.1854200001087,-0.0769762270984491,
4.41501595190525));
#19672=CARTESIAN_POINT('Ctrl Pts',(10.2101446228264,-0.293404201931947,
4.35739193013711));
#19673=CARTESIAN_POINT('Ctrl Pts',(10.2507745242318,-0.491764996345908,
4.00850959581219));
#19674=CARTESIAN_POINT('Ctrl Pts',(10.2984903602946,-0.273124940234581,
3.59096700393021));
#19675=CARTESIAN_POINT('Ctrl Pts',(10.3462061963575,0.196329951061554,3.54904570612073));
#19676=CARTESIAN_POINT('Ctrl Pts',(10.3939220324203,0.485492027373267,3.92124267520431));
#19677=CARTESIAN_POINT('Ctrl Pts',(10.4373868523273,0.34277731801193,4.32616121393696));
#19678=CARTESIAN_POINT('Ctrl Pts',(10.4649463935468,0.101188639822117,4.41483126760997));
#19679=CARTESIAN_POINT('Ctrl Pts',(10.4766006560786,-0.000378910032885704,
4.4157309619862));
#19680=CARTESIAN_POINT('Ctrl Pts',(10.2733993439214,5.73361663789851E-5,
4.41519339896199));
#19681=CARTESIAN_POINT('Ctrl Pts',(10.2817498797931,-0.0729553575157724,
4.41510384014646));
#19682=CARTESIAN_POINT('Ctrl Pts',(10.3060056943524,-0.285157432566911,
4.36192175935665));
#19683=CARTESIAN_POINT('Ctrl Pts',(10.3461667875993,-0.491301045992024,
4.02298928139638));
#19684=CARTESIAN_POINT('Ctrl Pts',(10.3938826236621,-0.285053227451061,
3.599188470261));
#19685=CARTESIAN_POINT('Ctrl Pts',(10.4415984597249,0.182963355965895,3.54345905416307));
#19686=CARTESIAN_POINT('Ctrl Pts',(10.4893142957878,0.482961874346273,3.9069782134126));
#19687=CARTESIAN_POINT('Ctrl Pts',(10.5332479238533,0.35082465130295,4.32033516829581));
#19688=CARTESIAN_POINT('Ctrl Pts',(10.5612762732311,0.105190355120073,4.41488124595214));
#19689=CARTESIAN_POINT('Ctrl Pts',(10.5733993439214,-0.000383826598418617,
4.41585315377736));
#19690=CARTESIAN_POINT('Origin',(3.42660065607856,0.,4.));
#19691=CARTESIAN_POINT('',(9.87660065607859,0.000332404019580576,4.41618417038907));
#19692=CARTESIAN_POINT('',(9.9733993439214,0.000362444897862246,4.41606425076498));
#19693=CARTESIAN_POINT('',(3.42660065607856,4.87367679877478E-13,4.415875));
#19694=CARTESIAN_POINT('Ctrl Pts',(9.87660065607859,0.000332404019580564,
4.41618417038907));
#19695=CARTESIAN_POINT('Ctrl Pts',(9.88998832798303,-0.116016130490024,
4.41516972706101));
#19696=CARTESIAN_POINT('Ctrl Pts',(9.91928127857509,-0.372296869871387,
4.30364082544554));
#19697=CARTESIAN_POINT('Ctrl Pts',(9.96447950785476,-0.474054618562381,
3.8689372536849));
#19698=CARTESIAN_POINT('Ctrl Pts',(10.0121953439176,-0.146148770628728,
3.53037700046135));
#19699=CARTESIAN_POINT('Ctrl Pts',(10.0599111799804,0.315967742161179,3.62307877379278));
#19700=CARTESIAN_POINT('Ctrl Pts',(10.1076270160433,0.487926215535836,4.06191310882887));
#19701=CARTESIAN_POINT('Ctrl Pts',(10.146523508076,0.262848409674369,4.37329037489646));
#19702=CARTESIAN_POINT('Ctrl Pts',(10.1695147214211,0.062069015396409,4.41538378814543));
#19703=CARTESIAN_POINT('Ctrl Pts',(10.1766006560786,0.000123197149224097,
4.41521991402453));
#19704=CARTESIAN_POINT('Ctrl Pts',(9.9733993439214,0.000362444897862267,
4.41606425076498));
#19705=CARTESIAN_POINT('Ctrl Pts',(9.9863182076674,-0.111995531308361,4.41503480155798));
#19706=CARTESIAN_POINT('Ctrl Pts',(10.015142350101,-0.364380386131072,4.30999810797653));
#19707=CARTESIAN_POINT('Ctrl Pts',(10.0598717712222,-0.477709011270712,
3.88295588266498));
#19708=CARTESIAN_POINT('Ctrl Pts',(10.1075876072851,-0.159916626226494,
3.53488507064564));
#19709=CARTESIAN_POINT('Ctrl Pts',(10.1553034433479,0.304729657315094,3.61393645496551));
#19710=CARTESIAN_POINT('Ctrl Pts',(10.2030192794107,0.489538007675758,4.04751593304174));
#19711=CARTESIAN_POINT('Ctrl Pts',(10.2423845796019,0.271127379494919,4.3692182851415));
#19712=CARTESIAN_POINT('Ctrl Pts',(10.2658446011055,0.0661120339180705,
4.41527442296197));
#19713=CARTESIAN_POINT('Ctrl Pts',(10.2733993439214,5.73361663789851E-5,
4.41519339896199));
#19714=CARTESIAN_POINT('Origin',(3.42660065607856,0.,4.));
#19715=CARTESIAN_POINT('',(9.57660065607859,-0.000290304052950346,4.41629504206998));
#19716=CARTESIAN_POINT('',(9.6733993439214,-0.000236899196693507,4.41639317328699));
#19717=CARTESIAN_POINT('',(3.42660065607856,4.87367679877478E-13,4.415875));
#19718=CARTESIAN_POINT('Ctrl Pts',(9.57660065607859,-0.000290304052950335,
4.41629504206998));
#19719=CARTESIAN_POINT('Ctrl Pts',(9.57865137716975,-0.0181001948149981,
4.41643644713422));
#19720=CARTESIAN_POINT('Ctrl Pts',(9.59660737694851,-0.173896467062472,
4.40729888742394));
#19721=CARTESIAN_POINT('Ctrl Pts',(9.63046865541489,-0.444448234747017,
4.21064422964382));
#19722=CARTESIAN_POINT('Ctrl Pts',(9.67818449147773,-0.41755432743774,3.74008922975375));
#19723=CARTESIAN_POINT('Ctrl Pts',(9.72590032754057,-0.00721385634321597,
3.50821428942208));
#19724=CARTESIAN_POINT('Ctrl Pts',(9.77361616360341,0.40975121003073,3.72795373420991));
#19725=CARTESIAN_POINT('Ctrl Pts',(9.82133199966624,0.450435435400681,4.19751745084266));
#19726=CARTESIAN_POINT('Ctrl Pts',(9.85566016382464,0.182118884769847,4.40484283743537));
#19727=CARTESIAN_POINT('Ctrl Pts',(9.87408304929542,0.0222122246324328,
4.41637494063069));
#19728=CARTESIAN_POINT('Ctrl Pts',(9.87660065607859,0.000332404019580564,
4.41618417038907));
#19729=CARTESIAN_POINT('Ctrl Pts',(9.6733993439214,-0.00023689919669354,
4.41639317328699));
#19730=CARTESIAN_POINT('Ctrl Pts',(9.67498125685411,-0.0139668454918635,
4.4164864708936));
#19731=CARTESIAN_POINT('Ctrl Pts',(9.69246844847443,-0.165649677201134,
4.40963259460397));
#19732=CARTESIAN_POINT('Ctrl Pts',(9.72586091878235,-0.438051576325333,
4.22364266437974));
#19733=CARTESIAN_POINT('Ctrl Pts',(9.77357675484519,-0.425028039486299,
3.75249971615691));
#19734=CARTESIAN_POINT('Ctrl Pts',(9.82129259090803,-0.0216947140899849,
3.50864008686857));
#19735=CARTESIAN_POINT('Ctrl Pts',(9.86900842697087,0.401561201071248,3.7160038263529));
#19736=CARTESIAN_POINT('Ctrl Pts',(9.91672426303371,0.456057286475463,4.18416562194019));
#19737=CARTESIAN_POINT('Ctrl Pts',(9.95152123535055,0.190383912560376,4.40224154849284));
#19738=CARTESIAN_POINT('Ctrl Pts',(9.97041292897978,0.0263359008882403,
4.4163022254471));
#19739=CARTESIAN_POINT('Ctrl Pts',(9.9733993439214,0.000362444897862267,
4.41606425076498));
#19740=CARTESIAN_POINT('Origin',(3.42660065607856,0.,4.));
#19741=CARTESIAN_POINT('',(9.27660065607858,-0.000185084181660103,4.41526520375254));
#19742=CARTESIAN_POINT('',(9.37339934392141,-0.000241596553487405,4.41532857883968));
#19743=CARTESIAN_POINT('',(3.42660065607856,4.87367679877478E-13,4.415875));
#19744=CARTESIAN_POINT('Ctrl Pts',(9.27660065607858,-0.000185084181660189,
4.41526520375254));
#19745=CARTESIAN_POINT('Ctrl Pts',(9.28321970504406,-0.0580335922681754,
4.4154966095816));
#19746=CARTESIAN_POINT('Ctrl Pts',(9.30574403269715,-0.254596444523232,
4.37718269734299));
#19747=CARTESIAN_POINT('Ctrl Pts',(9.34417363903789,-0.485900307124067,
4.07619787653679));
#19748=CARTESIAN_POINT('Ctrl Pts',(9.39188947510068,-0.326887306273347,
3.63250862071426));
#19749=CARTESIAN_POINT('Ctrl Pts',(9.43960531116356,0.13231133773591,3.52629235307153));
#19750=CARTESIAN_POINT('Ctrl Pts',(9.48732114722637,0.470006444430667,3.85508910653225));
#19751=CARTESIAN_POINT('Ctrl Pts',(9.53298626219807,0.380123833963086,4.29710958399465));
#19752=CARTESIAN_POINT('Ctrl Pts',(9.56274609848214,0.120032327051623,4.41533971732329));
#19753=CARTESIAN_POINT('Ctrl Pts',(9.57660065607859,-0.000290304052950335,
4.41629504206998));
#19754=CARTESIAN_POINT('Ctrl Pts',(9.3733993439214,-0.000241596553487357,
4.41532857883968));
#19755=CARTESIAN_POINT('Ctrl Pts',(9.37954958472843,-0.0539723465869793,
4.41561177485228));
#19756=CARTESIAN_POINT('Ctrl Pts',(9.40160510422307,-0.246305905820531,
4.3809303471886));
#19757=CARTESIAN_POINT('Ctrl Pts',(9.43956590240532,-0.483445357410111,
4.09047547319903));
#19758=CARTESIAN_POINT('Ctrl Pts',(9.48728173846818,-0.337568794959357,
3.64229546617122));
#19759=CARTESIAN_POINT('Ctrl Pts',(9.53499757453099,0.118302386066128,3.5226010365501));
#19760=CARTESIAN_POINT('Ctrl Pts',(9.58271341059386,0.465534665650901,3.84130942079228));
#19761=CARTESIAN_POINT('Ctrl Pts',(9.62884733372396,0.387920650713885,4.29034844530944));
#19762=CARTESIAN_POINT('Ctrl Pts',(9.65907597816649,0.124080336294106,4.41554841393524));
#19763=CARTESIAN_POINT('Ctrl Pts',(9.6733993439214,-0.00023689919669354,
4.41639317328699));
#19764=CARTESIAN_POINT('Origin',(3.42660065607856,0.,4.));
#19765=CARTESIAN_POINT('',(8.97660065607858,0.000361621133123973,4.41561526113518));
#19766=CARTESIAN_POINT('',(9.0733993439214,0.00033264130393823,4.41550825894961));
#19767=CARTESIAN_POINT('',(3.42660065607856,4.87367679877478E-13,4.415875));
#19768=CARTESIAN_POINT('Ctrl Pts',(8.97660065607858,0.000361621133123963,
4.41561526113518));
#19769=CARTESIAN_POINT('Ctrl Pts',(8.98778803291839,-0.097205817696177,
4.41480833810253));
#19770=CARTESIAN_POINT('Ctrl Pts',(9.01488068844582,-0.334723089553266,
4.33177224018802));
#19771=CARTESIAN_POINT('Ctrl Pts',(9.05787862266083,-0.487593182843731,
3.93551656882348));
#19772=CARTESIAN_POINT('Ctrl Pts',(9.10559445872368,-0.209472459465777,
3.55499829935456));
#19773=CARTESIAN_POINT('Ctrl Pts',(9.15331029478651,0.261010046587687,3.58313193881964));
#19774=CARTESIAN_POINT('Ctrl Pts',(9.20102613084934,0.491803010703882,3.99408193320625));
#19775=CARTESIAN_POINT('Ctrl Pts',(9.24212291794672,0.301599829163518,4.35270650246492));
#19776=CARTESIAN_POINT('Ctrl Pts',(9.26731442635645,0.0809737859182142,
4.41494055172187));
#19777=CARTESIAN_POINT('Ctrl Pts',(9.27660065607858,-0.000185084181660189,
4.41526520375254));
#19778=CARTESIAN_POINT('Ctrl Pts',(9.0733993439214,0.000332641303938268,
4.41550825894961));
#19779=CARTESIAN_POINT('Ctrl Pts',(9.08411791260276,-0.093207009794584,
4.4148098083896));
#19780=CARTESIAN_POINT('Ctrl Pts',(9.11074175997173,-0.326599857706223,
4.33721709571948));
#19781=CARTESIAN_POINT('Ctrl Pts',(9.1532708860283,-0.489280820139143,3.94990505119329));
#19782=CARTESIAN_POINT('Ctrl Pts',(9.20098672209113,-0.222487703095825,
3.56136068709803));
#19783=CARTESIAN_POINT('Ctrl Pts',(9.24870255815399,0.248619295113741,3.57562555337399));
#19784=CARTESIAN_POINT('Ctrl Pts',(9.29641839421681,0.49141536912078,3.97960000382683));
#19785=CARTESIAN_POINT('Ctrl Pts',(9.33798398947263,0.309808547095179,4.34782394055348));
#19786=CARTESIAN_POINT('Ctrl Pts',(9.36364430604082,0.0849819773478622,
4.41487939515448));
#19787=CARTESIAN_POINT('Ctrl Pts',(9.3733993439214,-0.000241596553487357,
4.41532857883968));
#19788=CARTESIAN_POINT('Origin',(3.42660065607856,0.,4.));
#19789=CARTESIAN_POINT('',(8.67660065607859,2.43999233753954E-5,4.41655967853978));
#19790=CARTESIAN_POINT('',(8.77339934392141,9.9565801791445E-5,4.41653262406943));
#19791=CARTESIAN_POINT('',(3.42660065607856,4.87367679877478E-13,4.415875));
#19792=CARTESIAN_POINT('Ctrl Pts',(8.67660065607859,2.43999233753836E-5,
4.41655967853978));
#19793=CARTESIAN_POINT('Ctrl Pts',(8.69235636079272,-0.136579453435425,
4.41644398151286));
#19794=CARTESIAN_POINT('Ctrl Pts',(8.72401734419445,-0.411298873006737,
4.26841067400337));
#19795=CARTESIAN_POINT('Ctrl Pts',(8.7715836062838,-0.449388340942622,3.80011167148426));
#19796=CARTESIAN_POINT('Ctrl Pts',(8.81929944234665,-0.0749173544856965,
3.51390061216986));
#19797=CARTESIAN_POINT('Ctrl Pts',(8.86701527840948,0.368351391347115,3.67408210030036));
#19798=CARTESIAN_POINT('Ctrl Pts',(8.91473111447233,0.473357386691186,4.13355901061654));
#19799=CARTESIAN_POINT('Ctrl Pts',(8.95125957369535,0.220969504140389,4.39141457480799));
#19800=CARTESIAN_POINT('Ctrl Pts',(8.97188275423077,0.0415074238114615,
4.41595555392421));
#19801=CARTESIAN_POINT('Ctrl Pts',(8.97660065607858,0.000361621133123963,
4.41561526113518));
#19802=CARTESIAN_POINT('Ctrl Pts',(8.77339934392141,9.95658017914599E-5,
4.41653262406943));
#19803=CARTESIAN_POINT('Ctrl Pts',(8.78868624047708,-0.132462770989084,
4.416105976883));
#19804=CARTESIAN_POINT('Ctrl Pts',(8.81987841572037,-0.403726445587972,
4.27580529254432));
#19805=CARTESIAN_POINT('Ctrl Pts',(8.86697586965126,-0.455080472922433,
3.81343369002772));
#19806=CARTESIAN_POINT('Ctrl Pts',(8.91469170571412,-0.0892013699275644,
3.51631793453238));
#19807=CARTESIAN_POINT('Ctrl Pts',(8.96240754177693,0.358592723611288,3.66337486216116));
#19808=CARTESIAN_POINT('Ctrl Pts',(9.0101233778398,0.477085601399612,4.11955983351088));
#19809=CARTESIAN_POINT('Ctrl Pts',(9.04712064522126,0.229261233371815,4.38814011953822));
#19810=CARTESIAN_POINT('Ctrl Pts',(9.06821263391514,0.0455964315317218,
4.41584623882512));
#19811=CARTESIAN_POINT('Ctrl Pts',(9.0733993439214,0.000332641303938268,
4.41550825894961));
#19812=CARTESIAN_POINT('Origin',(3.42660065607856,0.,4.));
#19813=CARTESIAN_POINT('',(8.37660065607859,-0.000374086211409503,4.41568853448753));
#19814=CARTESIAN_POINT('',(8.47339934392141,-0.000383538171196851,4.41580895574666));
#19815=CARTESIAN_POINT('',(3.42660065607856,4.87367679877478E-13,4.415875));
#19816=CARTESIAN_POINT('Ctrl Pts',(8.37660065607859,-0.000374086211409545,
4.41568853448753));
#19817=CARTESIAN_POINT('Ctrl Pts',(8.38101940997943,-0.0388937529272332,
4.41602262289185));
#19818=CARTESIAN_POINT('Ctrl Pts',(8.40134344256788,-0.215680110827853,
4.3934260635833));
#19819=CARTESIAN_POINT('Ctrl Pts',(8.43757275384394,-0.470763542849379,
4.14243212971755));
#19820=CARTESIAN_POINT('Ctrl Pts',(8.48528858990678,-0.37441192437669,3.68106280283335));
#19821=CARTESIAN_POINT('Ctrl Pts',(8.53300442596962,0.0657679253190804,
3.51257841158684));
#19822=CARTESIAN_POINT('Ctrl Pts',(8.58072026203246,0.445552077224736,3.79170076492532));
#19823=CARTESIAN_POINT('Ctrl Pts',(8.62843609809529,0.41617890091499,4.26210751092856));
#19824=CARTESIAN_POINT('Ctrl Pts',(8.66039622944401,0.140517691799823,4.41596716726027));
#19825=CARTESIAN_POINT('Ctrl Pts',(8.6764510821051,0.00132122424898086,
4.41656077688887));
#19826=CARTESIAN_POINT('Ctrl Pts',(8.67660065607859,2.43999233753836E-5,
4.41655967853978));
#19827=CARTESIAN_POINT('Ctrl Pts',(8.47339934392141,-0.000383538171196768,
4.41580895574666));
#19828=CARTESIAN_POINT('Ctrl Pts',(8.47734928966379,-0.0347911067166248,
4.41612244784963));
#19829=CARTESIAN_POINT('Ctrl Pts',(8.4972045140938,-0.207394442561863,4.39645832432586));
#19830=CARTESIAN_POINT('Ctrl Pts',(8.5329650172114,-0.466364439759318,4.15623518867385));
#19831=CARTESIAN_POINT('Ctrl Pts',(8.58068085327425,-0.383642787608637,
3.69222827230584));
#19832=CARTESIAN_POINT('Ctrl Pts',(8.62839668933707,0.0513839395061145,
3.51085286915611));
#19833=CARTESIAN_POINT('Ctrl Pts',(8.67611252539993,0.439224004328866,3.77866880275638));
#19834=CARTESIAN_POINT('Ctrl Pts',(8.72382836146275,0.42371790764641,4.24973658040369));
#19835=CARTESIAN_POINT('Ctrl Pts',(8.75625730096992,0.148732406864234,4.41402322426773));
#19836=CARTESIAN_POINT('Ctrl Pts',(8.77278096178947,0.00546194790078228,
4.41654988270631));
#19837=CARTESIAN_POINT('Ctrl Pts',(8.77339934392141,9.95658017914599E-5,
4.41653262406943));
#19838=CARTESIAN_POINT('Origin',(3.42660065607856,0.,4.));
#19839=CARTESIAN_POINT('',(8.07660065607859,0.000145957947245773,4.41523406184916));
#19840=CARTESIAN_POINT('',(8.1733993439214,8.12049300508987E-5,4.41520065480005));
#19841=CARTESIAN_POINT('',(3.42660065607856,4.87367679877478E-13,4.415875));
#19842=CARTESIAN_POINT('Ctrl Pts',(8.07660065607858,0.00014595794724577,
4.41523406184916));
#19843=CARTESIAN_POINT('Ctrl Pts',(8.08558773785375,-0.0784131624224431,
4.41498734772332));
#19844=CARTESIAN_POINT('Ctrl Pts',(8.11048009831652,-0.296350794919178,
4.35572875890285));
#19845=CARTESIAN_POINT('Ctrl Pts',(8.15127773746691,-0.491827368180951,
4.00332637343646));
#19846=CARTESIAN_POINT('Ctrl Pts',(8.19899357352975,-0.268798940774433,
3.58811123553743));
#19847=CARTESIAN_POINT('Ctrl Pts',(8.24670940959259,0.201071689948468,3.55113988776764));
#19848=CARTESIAN_POINT('Ctrl Pts',(8.29442524565542,0.486295093906121,3.92636368766143));
#19849=CARTESIAN_POINT('Ctrl Pts',(8.33772232781743,0.339888039743562,4.32819890206972));
#19850=CARTESIAN_POINT('Ctrl Pts',(8.36511413129181,0.0997575609540166,
4.41482007364463));
#19851=CARTESIAN_POINT('Ctrl Pts',(8.37660065607859,-0.000374086211409545,
4.41568853448753));
#19852=CARTESIAN_POINT('Ctrl Pts',(8.1733993439214,8.12049300509751E-5,
4.41520065480005));
#19853=CARTESIAN_POINT('Ctrl Pts',(8.18191761753811,-0.0743948540356096,
4.41507113968239));
#19854=CARTESIAN_POINT('Ctrl Pts',(8.20634116984244,-0.288109900049694,
4.36032095112539));
#19855=CARTESIAN_POINT('Ctrl Pts',(8.24667000083438,-0.491516046133,4.01781014446235));
#19856=CARTESIAN_POINT('Ctrl Pts',(8.29438583689722,-0.280813212199106,
3.59620653211525));
#19857=CARTESIAN_POINT('Ctrl Pts',(8.34210167296004,0.187764715363875,3.54541267448783));
#19858=CARTESIAN_POINT('Ctrl Pts',(8.38981750902289,0.483915415676709,3.91207335260334));
#19859=CARTESIAN_POINT('Ctrl Pts',(8.43358339934334,0.347950231939931,4.32244196179047));
#19860=CARTESIAN_POINT('Ctrl Pts',(8.46144401097618,0.1037581297464,4.41486010664565));
#19861=CARTESIAN_POINT('Ctrl Pts',(8.47339934392141,-0.000383538171196768,
4.41580895574666));
#19862=CARTESIAN_POINT('Origin',(3.42660065607856,0.,4.));
#19863=CARTESIAN_POINT('',(7.77660065607858,0.000318631424802313,4.41622521972442));
#19864=CARTESIAN_POINT('',(7.8733993439214,0.000353153796088606,4.4161078667978));
#19865=CARTESIAN_POINT('',(3.42660065607856,4.87367679877478E-13,4.415875));
#19866=CARTESIAN_POINT('Ctrl Pts',(7.77660065607859,0.000318631424802297,
4.41622521972442));
#19867=CARTESIAN_POINT('Ctrl Pts',(7.79015606572807,-0.117457481003694,
4.41522659035305));
#19868=CARTESIAN_POINT('Ctrl Pts',(7.81961675406517,-0.375115671948731,
4.30131743988157));
#19869=CARTESIAN_POINT('Ctrl Pts',(7.86498272108989,-0.472647010158531,
3.86394843388276));
#19870=CARTESIAN_POINT('Ctrl Pts',(7.91269855715272,-0.141191260335066,
3.52886280888004));
#19871=CARTESIAN_POINT('Ctrl Pts',(7.96041439321556,0.31992259635559,3.62642971585976));
#19872=CARTESIAN_POINT('Ctrl Pts',(8.0081302292784,0.48724661017382,4.0670519628834));
#19873=CARTESIAN_POINT('Ctrl Pts',(8.04685898356608,0.259884401562094,4.37470733986759));
#19874=CARTESIAN_POINT('Ctrl Pts',(8.06968245916614,0.0606202562326388,
4.41542398077349));
#19875=CARTESIAN_POINT('Ctrl Pts',(8.07660065607858,0.00014595794724577,
4.41523406184916));
#19876=CARTESIAN_POINT('Ctrl Pts',(7.8733993439214,0.000353153796088627,
4.4161078667978));
#19877=CARTESIAN_POINT('Ctrl Pts',(7.88648594541244,-0.113432877329791,
4.41507910421771));
#19878=CARTESIAN_POINT('Ctrl Pts',(7.9154778255911,-0.367219156371593,4.30774647947464));
#19879=CARTESIAN_POINT('Ctrl Pts',(7.96037498445733,-0.476448943335793,
3.87792777037096));
#19880=CARTESIAN_POINT('Ctrl Pts',(8.0080908205202,-0.1550058622045,3.53322552818936));
#19881=CARTESIAN_POINT('Ctrl Pts',(8.05580665658301,0.308781487260178,3.61716946571973));
#19882=CARTESIAN_POINT('Ctrl Pts',(8.10352249264587,0.489010045760349,4.0526725734847));
#19883=CARTESIAN_POINT('Ctrl Pts',(8.14272005509199,0.26816615642074,4.37069430501912));
#19884=CARTESIAN_POINT('Ctrl Pts',(8.1660123388505,0.064666477720629,4.4153129696744));
#19885=CARTESIAN_POINT('Ctrl Pts',(8.1733993439214,8.12049300509751E-5,
4.41520065480005));
#19886=CARTESIAN_POINT('Origin',(3.42660065607856,0.,4.));
#19887=CARTESIAN_POINT('',(7.47660065607859,-0.000306770237538029,4.41625647512786));
#19888=CARTESIAN_POINT('',(7.5733993439214,-0.000257198714157858,4.41635988094829));
#19889=CARTESIAN_POINT('',(3.42660065607856,4.87367679877478E-13,4.415875));
#19890=CARTESIAN_POINT('Ctrl Pts',(7.47660065607859,-0.00030677023753798,
4.41625647512786));
#19891=CARTESIAN_POINT('Ctrl Pts',(7.47881911491479,-0.0195780710793754,
4.41641565502598));
#19892=CARTESIAN_POINT('Ctrl Pts',(7.4969428524386,-0.176849480241104,4.4064317922735));
#19893=CARTESIAN_POINT('Ctrl Pts',(7.53097186865002,-0.44664354691983,4.20594845626764));
#19894=CARTESIAN_POINT('Ctrl Pts',(7.57868770471286,-0.414791917646955,
3.73570302684109));
#19895=CARTESIAN_POINT('Ctrl Pts',(7.62640354077569,-0.00203048755240202,
3.50816557464413));
#19896=CARTESIAN_POINT('Ctrl Pts',(7.67411937683853,0.412595570264971,3.73228724307244));
#19897=CARTESIAN_POINT('Ctrl Pts',(7.72183521290137,0.448328767436039,4.20225365549051));
#19898=CARTESIAN_POINT('Ctrl Pts',(7.75599563931472,0.179163779268806,4.40574053813273));
#19899=CARTESIAN_POINT('Ctrl Pts',(7.77425078704046,0.0207354574140521,
4.41639833498254));
#19900=CARTESIAN_POINT('Ctrl Pts',(7.77660065607859,0.000318631424802297,
4.41622521972442));
#19901=CARTESIAN_POINT('Ctrl Pts',(7.5733993439214,-0.000257198714157839,
4.41635988094829));
#19902=CARTESIAN_POINT('Ctrl Pts',(7.57514899459915,-0.0154461882200338,
4.41646996636401));
#19903=CARTESIAN_POINT('Ctrl Pts',(7.59280392396451,-0.168599214901356,
4.40881268721627));
#19904=CARTESIAN_POINT('Ctrl Pts',(7.62636413201748,-0.440384235482588,
4.21901358396786));
#19905=CARTESIAN_POINT('Ctrl Pts',(7.67407996808031,-0.422396009600076,
3.7480340579683));
#19906=CARTESIAN_POINT('Ctrl Pts',(7.72179580414317,-0.0165150286377962,
3.50843873354525));
#19907=CARTESIAN_POINT('Ctrl Pts',(7.76951164020598,0.404531957204003,3.72025168374225));
#19908=CARTESIAN_POINT('Ctrl Pts',(7.81722747626884,0.454091022239626,4.18896181724392));
#19909=CARTESIAN_POINT('Ctrl Pts',(7.85185671084063,0.187425762196077,4.40318800700955));
#19910=CARTESIAN_POINT('Ctrl Pts',(7.87058066672482,0.02486112795907,4.41632944836175));
#19911=CARTESIAN_POINT('Ctrl Pts',(7.8733993439214,0.000353153796088627,
4.4161078667978));
#19912=CARTESIAN_POINT('Origin',(3.42660065607856,0.,4.));
#19913=CARTESIAN_POINT('',(7.17660065607858,-0.000163391746992416,4.4152468210878));
#19914=CARTESIAN_POINT('',(7.2733993439214,-0.000222139526412562,4.4153039283715));
#19915=CARTESIAN_POINT('',(3.42660065607856,4.87367679877478E-13,4.415875));
#19916=CARTESIAN_POINT('Ctrl Pts',(7.17660065607859,-0.000163391746992363,
4.4152468210878));
#19917=CARTESIAN_POINT('Ctrl Pts',(7.18338744278911,-0.0594844418834033,
4.41545575762517));
#19918=CARTESIAN_POINT('Ctrl Pts',(7.20607950818724,-0.257561782965025,
4.37580284351512));
#19919=CARTESIAN_POINT('Ctrl Pts',(7.24467685227299,-0.486676365692783,
4.07107270446015));
#19920=CARTESIAN_POINT('Ctrl Pts',(7.29239268833582,-0.322996137187983,
3.62908393881966));
#19921=CARTESIAN_POINT('Ctrl Pts',(7.34010852439867,0.137296434535941,3.52771310152703));
#19922=CARTESIAN_POINT('Ctrl Pts',(7.3878243604615,0.471507566988788,3.86005058906394));
#19923=CARTESIAN_POINT('Ctrl Pts',(7.43332173768814,0.377318713751663,4.29947917201381));
#19924=CARTESIAN_POINT('Ctrl Pts',(7.46291383622717,0.118587850938607,4.41527441201542));
#19925=CARTESIAN_POINT('Ctrl Pts',(7.47660065607859,-0.00030677023753798,
4.41625647512786));
#19926=CARTESIAN_POINT('Ctrl Pts',(7.2733993439214,-0.000222139526412493,
4.4153039283715));
#19927=CARTESIAN_POINT('Ctrl Pts',(7.27971732247348,-0.0554265094472961,
4.41557047734173));
#19928=CARTESIAN_POINT('Ctrl Pts',(7.30194057971316,-0.249272617462211,
4.37960776139715));
#19929=CARTESIAN_POINT('Ctrl Pts',(7.34006911564044,-0.484372034479295,
4.08537538031203));
#19930=CARTESIAN_POINT('Ctrl Pts',(7.3877849517033,-0.333780171974684,3.63875766810317));
#19931=CARTESIAN_POINT('Ctrl Pts',(7.43550078776612,0.123327161313159,3.52387434835784));
#19932=CARTESIAN_POINT('Ctrl Pts',(7.48321662382897,0.467181263150904,3.84622454030349));
#19933=CARTESIAN_POINT('Ctrl Pts',(7.52918280921405,0.385138488472668,4.29279105563264));
#19934=CARTESIAN_POINT('Ctrl Pts',(7.55924371591154,0.122630008444172,4.41546922990911));
#19935=CARTESIAN_POINT('Ctrl Pts',(7.5733993439214,-0.000257198714157839,
4.41635988094829));
#19936=CARTESIAN_POINT('Origin',(3.42660065607856,0.,4.));
#19937=CARTESIAN_POINT('',(6.87660065607859,0.000369753976522709,4.4156559906262));
#19938=CARTESIAN_POINT('',(6.9733993439214,0.000344359613660638,4.41554532105972));
#19939=CARTESIAN_POINT('',(3.42660065607856,4.87367679877478E-13,4.415875));
#19940=CARTESIAN_POINT('Ctrl Pts',(6.87660065607859,0.000369753976522759,
4.4156559906262));
#19941=CARTESIAN_POINT('Ctrl Pts',(6.88795577066343,-0.0986361616094132,
4.41481368816743));
#19942=CARTESIAN_POINT('Ctrl Pts',(6.91521616393589,-0.337621850525623,
4.32977807754403));
#19943=CARTESIAN_POINT('Ctrl Pts',(6.95838183589596,-0.486886005735063,
3.93038141845316));
#19944=CARTESIAN_POINT('Ctrl Pts',(7.0060976719588,-0.204771183672361,3.55281534000283));
#19945=CARTESIAN_POINT('Ctrl Pts',(7.05381350802163,0.265389096458903,3.58590591031157));
#19946=CARTESIAN_POINT('Ctrl Pts',(7.10152934408448,0.491837993618785,3.99926540470374));
#19947=CARTESIAN_POINT('Ctrl Pts',(7.14245839343679,0.298657604039877,4.35441002681052));
#19948=CARTESIAN_POINT('Ctrl Pts',(7.16748216410149,0.0795383202432945,
4.41496610118));
#19949=CARTESIAN_POINT('Ctrl Pts',(7.17660065607859,-0.000163391746992363,
4.4152468210878));
#19950=CARTESIAN_POINT('Ctrl Pts',(6.9733993439214,0.00034435961366068,
4.41554532105972));
#19951=CARTESIAN_POINT('Ctrl Pts',(6.9842856503478,-0.0946377878655052,
4.41480662962373));
#19952=CARTESIAN_POINT('Ctrl Pts',(7.0110772354618,-0.329510302625179,4.33529054280597));
#19953=CARTESIAN_POINT('Ctrl Pts',(7.05377409926342,-0.488725618924084,
3.94475128051735));
#19954=CARTESIAN_POINT('Ctrl Pts',(7.10148993532626,-0.21785253135038,3.55904022429238));
#19955=CARTESIAN_POINT('Ctrl Pts',(7.14920577138909,0.253078023397415,3.57826934481931));
#19956=CARTESIAN_POINT('Ctrl Pts',(7.19692160745195,0.491603063369337,3.98478019943955));
#19957=CARTESIAN_POINT('Ctrl Pts',(7.2383194649627,0.306874094293292,4.34959156107453));
#19958=CARTESIAN_POINT('Ctrl Pts',(7.26381204378586,0.0835484619188193,
4.41489945011039));
#19959=CARTESIAN_POINT('Ctrl Pts',(7.2733993439214,-0.000222139526412493,
4.4153039283715));
#19960=CARTESIAN_POINT('Origin',(3.42660065607856,0.,4.));
#19961=CARTESIAN_POINT('',(6.57660065607858,1.8302248101926E-5,4.41656360501758));
#19962=CARTESIAN_POINT('',(6.6733993439214,7.63499956435865E-5,4.4165465803965));
#19963=CARTESIAN_POINT('',(3.42660065607856,4.87367679877478E-13,4.415875));
#19964=CARTESIAN_POINT('Ctrl Pts',(6.57660065607858,1.83022481018748E-5,
4.41656360501758));
#19965=CARTESIAN_POINT('Ctrl Pts',(6.57661881985014,-0.000139156870309867,
4.41656362372179));
#19966=CARTESIAN_POINT('Ctrl Pts',(6.59254226230931,-0.138177237712184,
4.41649399470799));
#19967=CARTESIAN_POINT('Ctrl Pts',(6.62437098345609,-0.41404349770976,4.26553045144514));
#19968=CARTESIAN_POINT('Ctrl Pts',(6.67208681951894,-0.447234019333667,
3.79538894860702));
#19969=CARTESIAN_POINT('Ctrl Pts',(6.71980265558177,-0.0698021891909718,
3.51313682319347));
#19970=CARTESIAN_POINT('Ctrl Pts',(6.76751849164461,0.371772181936036,3.67798293440124));
#19971=CARTESIAN_POINT('Ctrl Pts',(6.81523432770745,0.471920133146607,4.13853999974893));
#19972=CARTESIAN_POINT('Ctrl Pts',(6.85159504918544,0.21800401543618,4.39254992240466));
#19973=CARTESIAN_POINT('Ctrl Pts',(6.87205049197582,0.0400429038769189,
4.41599351380864));
#19974=CARTESIAN_POINT('Ctrl Pts',(6.87660065607859,0.000369753976522759,
4.4156559906262));
#19975=CARTESIAN_POINT('Ctrl Pts',(6.6733993439214,7.63499956435956E-5,
4.4165465803965));
#19976=CARTESIAN_POINT('Ctrl Pts',(6.68885397822212,-0.133927014866661,
4.41622291450327));
#19977=CARTESIAN_POINT('Ctrl Pts',(6.72021389121046,-0.406451392834186,
4.27318229388465));
#19978=CARTESIAN_POINT('Ctrl Pts',(6.76747908288639,-0.453085647428837,
3.80864864857145));
#19979=CARTESIAN_POINT('Ctrl Pts',(6.81519491894923,-0.0841006081168706,
3.51540431248109));
#19980=CARTESIAN_POINT('Ctrl Pts',(6.86291075501207,0.362121456530253,3.66717299786736));
#19981=CARTESIAN_POINT('Ctrl Pts',(6.91062659107491,0.475798562415156,4.124581128109));
#19982=CARTESIAN_POINT('Ctrl Pts',(6.94745612071136,0.226294304474162,4.38932900794447));
#19983=CARTESIAN_POINT('Ctrl Pts',(6.96838037166019,0.0441344886838037,
4.41588588393584));
#19984=CARTESIAN_POINT('Ctrl Pts',(6.9733993439214,0.00034435961366068,
4.41554532105972));
#19985=CARTESIAN_POINT('Origin',(3.42660065607856,0.,4.));
#19986=CARTESIAN_POINT('',(6.27660065607859,-8.94903747701068E-6,4.41582842213685));
#19987=CARTESIAN_POINT('',(6.3733993439214,-0.000441664590319634,4.4157663968931));
#19988=CARTESIAN_POINT('',(3.42660065607856,4.87367679877478E-13,4.415875));
#19989=CARTESIAN_POINT('Ctrl Pts',(6.27660065607859,-8.94903747701223E-6,
4.41582842213685));
#19990=CARTESIAN_POINT('Ctrl Pts',(6.28118714772447,-0.0399801639742102,
4.41579747358059));
#19991=CARTESIAN_POINT('Ctrl Pts',(6.29372627871415,-0.149263049162913,
4.40013952362907));
#19992=CARTESIAN_POINT('Ctrl Pts',(6.31421804904765,-0.307151379675736,
4.3060270879454));
#19993=CARTESIAN_POINT('Ctrl Pts',(6.33807596707907,-0.416657206472865,
4.12081787696614));
#19994=CARTESIAN_POINT('Ctrl Pts',(6.36193388511048,-0.422829889105799,
3.9075587958503));
#19995=CARTESIAN_POINT('Ctrl Pts',(6.39374444248571,-0.296437506874183,
3.64987069373525));
#19996=CARTESIAN_POINT('Ctrl Pts',(6.43350763920474,0.0703302468340302,
3.51324810367198));
#19997=CARTESIAN_POINT('Ctrl Pts',(6.48122347526758,0.448014600657906,3.7964368525222));
#19998=CARTESIAN_POINT('Ctrl Pts',(6.52892114755886,0.413253290380966,4.26628466471864));
#19999=CARTESIAN_POINT('Ctrl Pts',(6.56071354116253,0.137741412285014,4.41654724519979));
#20000=CARTESIAN_POINT('Ctrl Pts',(6.57660065607858,1.83022481018748E-5,
4.41656360501758));
#20001=CARTESIAN_POINT('Ctrl Pts',(6.3733993439214,-0.000441664590319611,
4.4157663968931));
#20002=CARTESIAN_POINT('Ctrl Pts',(6.37751702740883,-0.0362476131304844,
4.41610293027605));
#20003=CARTESIAN_POINT('Ctrl Pts',(6.39753998958387,-0.210006484715375,
4.39546152579387));
#20004=CARTESIAN_POINT('Ctrl Pts',(6.43346823044653,-0.468271923807345,
4.15124960425567));
#20005=CARTESIAN_POINT('Ctrl Pts',(6.48118406650937,-0.380227249479543,
3.6882349865083));
#20006=CARTESIAN_POINT('Ctrl Pts',(6.52889990257221,0.0564566449812287,
3.51140415777354));
#20007=CARTESIAN_POINT('Ctrl Pts',(6.57661573863504,0.441574375138847,3.78331933667001));
#20008=CARTESIAN_POINT('Ctrl Pts',(6.62433157469789,0.421040068198854,4.25418342072721));
#20009=CARTESIAN_POINT('Ctrl Pts',(6.65659277646,0.145792717270209,4.41473316952435));
#20010=CARTESIAN_POINT('Ctrl Pts',(6.6729486995345,0.00398377756883227,
4.41655601822694));
#20011=CARTESIAN_POINT('Ctrl Pts',(6.6733993439214,7.63499956435956E-5,
4.4165465803965));
#20012=CARTESIAN_POINT('Origin',(3.42660065607856,0.,4.));
#20013=CARTESIAN_POINT('',(5.97660065607859,-9.19412645702589E-6,4.41589218083175));
#20014=CARTESIAN_POINT('',(6.0733993439214,-6.65563173402051E-6,4.41590255337155));
#20015=CARTESIAN_POINT('',(3.42660065607856,4.87367679877478E-13,4.415875));
#20016=CARTESIAN_POINT('Ctrl Pts',(5.97660065607858,-9.19412645705893E-6,
4.41589218083175));
#20017=CARTESIAN_POINT('Ctrl Pts',(5.97780283625498,-0.0104787976275591,
4.4159022685469));
#20018=CARTESIAN_POINT('Ctrl Pts',(5.98695765577519,-0.0902010538040918,
4.41295272969856));
#20019=CARTESIAN_POINT('Ctrl Pts',(6.0040651146392,-0.23587461323539,4.36380751861078));
#20020=CARTESIAN_POINT('Ctrl Pts',(6.02792303267061,-0.381351759249696,
4.20630938167977));
#20021=CARTESIAN_POINT('Ctrl Pts',(6.05178095070204,-0.433578399193506,
3.9983625870902));
#20022=CARTESIAN_POINT('Ctrl Pts',(6.07563886873346,-0.379782579589031,
3.79081692866841));
#20023=CARTESIAN_POINT('Ctrl Pts',(6.09949678676487,-0.233120953551068,
3.63442082419035));
#20024=CARTESIAN_POINT('Ctrl Pts',(6.12335470479629,-0.0294522997972467,
3.5674214393556));
#20025=CARTESIAN_POINT('Ctrl Pts',(6.14721262282771,0.181413325723775,3.60619428643423));
#20026=CARTESIAN_POINT('Ctrl Pts',(6.17107054085913,0.347927737305898,3.74127281623538));
#20027=CARTESIAN_POINT('Ctrl Pts',(6.19492845889055,0.429346806292137,3.93959933010928));
#20028=CARTESIAN_POINT('Ctrl Pts',(6.21878637692197,0.405811992579865,4.15272917617017));
#20029=CARTESIAN_POINT('Ctrl Pts',(6.24264429495339,0.282982581651336,4.32844890303245));
#20030=CARTESIAN_POINT('Ctrl Pts',(6.26191572133893,0.127967070080381,4.40561019629887));
#20031=CARTESIAN_POINT('Ctrl Pts',(6.27323450838066,0.029326984292613,4.415851136102));
#20032=CARTESIAN_POINT('Ctrl Pts',(6.27660065607859,-8.94903747701223E-6,
4.41582842213685));
#20033=CARTESIAN_POINT('Ctrl Pts',(6.0733993439214,-6.65563173397714E-6,
4.41590255337156));
#20034=CARTESIAN_POINT('Ctrl Pts',(6.07413271593935,-0.00639299139291402,
4.41590724351385));
#20035=CARTESIAN_POINT('Ctrl Pts',(6.0828187273011,-0.0820297780542147,
4.41420140028919));
#20036=CARTESIAN_POINT('Ctrl Pts',(6.09945737800665,-0.2250554921608,4.3705991908187));
#20037=CARTESIAN_POINT('Ctrl Pts',(6.12331529603809,-0.375113923638194,
4.21744656883549));
#20038=CARTESIAN_POINT('Ctrl Pts',(6.1471732140695,-0.433431396087355,4.01114207710762));
#20039=CARTESIAN_POINT('Ctrl Pts',(6.17103113210093,-0.385792139046387,
3.80207577201042));
#20040=CARTESIAN_POINT('Ctrl Pts',(6.19488905013233,-0.243761337718234,
3.64147770828707));
#20041=CARTESIAN_POINT('Ctrl Pts',(6.21874696816376,-0.042227823444436,
3.56841523311022));
#20042=CARTESIAN_POINT('Ctrl Pts',(6.24260488619517,0.16982704650124,3.60113783246665));
#20043=CARTESIAN_POINT('Ctrl Pts',(6.2664628042266,0.339985970990829,3.73091992247201));
#20044=CARTESIAN_POINT('Ctrl Pts',(6.29032072225801,0.427700638223926,3.92738904240251));
#20045=CARTESIAN_POINT('Ctrl Pts',(6.31417864028943,0.409561128158778,4.13996490148311));
#20046=CARTESIAN_POINT('Ctrl Pts',(6.34187151417723,0.27471212230801,4.35031587281991));
#20047=CARTESIAN_POINT('Ctrl Pts',(6.36161174872122,0.102059178040878,4.41480301073152));
#20048=CARTESIAN_POINT('Ctrl Pts',(6.3733993439214,-0.000441664590319611,
4.4157663968931));
#20049=CARTESIAN_POINT('Origin',(3.42660065607856,0.,4.));
#20050=CARTESIAN_POINT('',(5.67660065607858,1.06631253201556E-5,4.41586554077139));
#20051=CARTESIAN_POINT('',(5.7733993439214,9.17748676071416E-6,4.4158542849441));
#20052=CARTESIAN_POINT('',(3.42660065607856,4.87367679877478E-13,4.415875));
#20053=CARTESIAN_POINT('Ctrl Pts',(5.67660065607858,1.06631253201268E-5,
4.41586554077139));
#20054=CARTESIAN_POINT('Ctrl Pts',(5.68237116412931,-0.050253077703417,
4.41581669384736));
#20055=CARTESIAN_POINT('Ctrl Pts',(5.69609431152383,-0.169828933264711,
4.3941204493343));
#20056=CARTESIAN_POINT('Ctrl Pts',(5.71777009826218,-0.329222253834466,
4.28214440376531));
#20057=CARTESIAN_POINT('Ctrl Pts',(5.74162801629359,-0.424158110434281,
4.08990358344764));
#20058=CARTESIAN_POINT('Ctrl Pts',(5.76548593432501,-0.415375755386326,
3.8756788878607));
#20059=CARTESIAN_POINT('Ctrl Pts',(5.78934385235642,-0.305022713182347,
3.69185409099321));
#20060=CARTESIAN_POINT('Ctrl Pts',(5.81320177038785,-0.120083309624962,
3.58337936191985));
#20061=CARTESIAN_POINT('Ctrl Pts',(5.83705968841926,0.0942197354074567,
3.57677972866706));
#20062=CARTESIAN_POINT('Ctrl Pts',(5.86091760645069,0.285483486244351,3.673668977605));
#20063=CARTESIAN_POINT('Ctrl Pts',(5.8847755244821,0.406938752801468,3.85035505520226));
#20064=CARTESIAN_POINT('Ctrl Pts',(5.90863344251353,0.428886400972996,4.06363338935351));
#20065=CARTESIAN_POINT('Ctrl Pts',(5.93249136054494,0.345959657594393,4.261351642888));
#20066=CARTESIAN_POINT('Ctrl Pts',(5.95514709839996,0.186877681905787,4.38841966610496));
#20067=CARTESIAN_POINT('Ctrl Pts',(5.96985019691118,0.0587795235055939,
4.41583553648629));
#20068=CARTESIAN_POINT('Ctrl Pts',(5.97660065607858,-9.19412645705893E-6,
4.41589218083175));
#20069=CARTESIAN_POINT('Ctrl Pts',(5.7733993439214,9.17748676073846E-6,
4.4158542849441));
#20070=CARTESIAN_POINT('Ctrl Pts',(5.77870104381367,-0.0461746181927863,
4.41581721944429));
#20071=CARTESIAN_POINT('Ctrl Pts',(5.79195538304975,-0.161664917198308,
4.3966319946429));
#20072=CARTESIAN_POINT('Ctrl Pts',(5.81316236162963,-0.320769768688322,
4.29171820750724));
#20073=CARTESIAN_POINT('Ctrl Pts',(5.83702027966105,-0.421326288178809,
4.10235681181338));
#20074=CARTESIAN_POINT('Ctrl Pts',(5.86087819769247,-0.418857046020503,
3.88796639709818));
#20075=CARTESIAN_POINT('Ctrl Pts',(5.88473611572389,-0.313965860818636,
3.70097123187977));
#20076=CARTESIAN_POINT('Ctrl Pts',(5.90859403375531,-0.132301443679057,
3.58709678011166));
#20077=CARTESIAN_POINT('Ctrl Pts',(5.93245195178673,0.0817142298265842,
3.57418834816524));
#20078=CARTESIAN_POINT('Ctrl Pts',(5.95630986981814,0.275748643515392,3.66540258613358));
#20079=CARTESIAN_POINT('Ctrl Pts',(5.98016778784957,0.402354822815078,3.83843477537114));
#20080=CARTESIAN_POINT('Ctrl Pts',(6.00402570588098,0.430574627524036,4.05097449853386));
#20081=CARTESIAN_POINT('Ctrl Pts',(6.02788362391241,0.353506566116634,4.25104874587108));
#20082=CARTESIAN_POINT('Ctrl Pts',(6.05100816992587,0.195023852357142,4.38547315270063));
#20083=CARTESIAN_POINT('Ctrl Pts',(6.06618007659554,0.06286002589468,4.4158563839102));
#20084=CARTESIAN_POINT('Ctrl Pts',(6.0733993439214,-6.65563173397714E-6,
4.41590255337156));
#20085=CARTESIAN_POINT('Origin',(3.42660065607856,0.,4.));
#20086=CARTESIAN_POINT('',(5.37660065607858,-1.01751121954902E-5,4.41586038335289));
#20087=CARTESIAN_POINT('',(5.4733993439214,-1.09014992595302E-5,4.41587264340464));
#20088=CARTESIAN_POINT('',(3.42660065607856,4.87367679877478E-13,4.415875));
#20089=CARTESIAN_POINT('Ctrl Pts',(5.37660065607859,-1.01751121954468E-5,
4.41586038335289));
#20090=CARTESIAN_POINT('Ctrl Pts',(5.37898685265982,-0.0207957689391596,
4.41587928195339));
#20091=CARTESIAN_POINT('Ctrl Pts',(5.38932568858487,-0.110842971866809,
4.40924760552439));
#20092=CARTESIAN_POINT('Ctrl Pts',(5.40761716385372,-0.26226226804932,4.34526983614494));
#20093=CARTESIAN_POINT('Ctrl Pts',(5.43147508188515,-0.395631058815178,
4.17739453851434));
#20094=CARTESIAN_POINT('Ctrl Pts',(5.45533299991656,-0.432257278927009,
3.96614144408682));
#20095=CARTESIAN_POINT('Ctrl Pts',(5.47919091794798,-0.363184819889405,
3.76316768886851));
#20096=CARTESIAN_POINT('Ctrl Pts',(5.5030488359794,-0.205303779432806,3.61810588490468));
#20097=CARTESIAN_POINT('Ctrl Pts',(5.52690675401082,0.00277962745745752,
3.56642759466814));
#20098=CARTESIAN_POINT('Ctrl Pts',(5.55076467204224,0.210183339719457,3.62076956781107));
#20099=CARTESIAN_POINT('Ctrl Pts',(5.57462259007365,0.36619150013966,3.76784371165257));
#20100=CARTESIAN_POINT('Ctrl Pts',(5.59848050810508,0.432655863921731,3.97168639180759));
#20101=CARTESIAN_POINT('Ctrl Pts',(5.62233842613649,0.393324083661671,4.18245252040861));
#20102=CARTESIAN_POINT('Ctrl Pts',(5.64619634416792,0.257813851021257,4.34860403787086));
#20103=CARTESIAN_POINT('Ctrl Pts',(5.66428375414861,0.107285005985459,4.40994309575933));
#20104=CARTESIAN_POINT('Ctrl Pts',(5.6744185247855,0.0190180158238588,4.41588401235146));
#20105=CARTESIAN_POINT('Ctrl Pts',(5.67660065607858,1.06631253201268E-5,
4.41586554077139));
#20106=CARTESIAN_POINT('Ctrl Pts',(5.4733993439214,-1.0901499259525E-5,
4.41587264340464));
#20107=CARTESIAN_POINT('Ctrl Pts',(5.47531673234419,-0.0167114040746605,
4.41588973972128));
#20108=CARTESIAN_POINT('Ctrl Pts',(5.48518676011079,-0.102669266038577,
4.41080986982701));
#20109=CARTESIAN_POINT('Ctrl Pts',(5.50300942722118,-0.251979671819092,
4.35284416104532));
#20110=CARTESIAN_POINT('Ctrl Pts',(5.52686734525261,-0.390234841353927,
4.18896964197264));
#20111=CARTESIAN_POINT('Ctrl Pts',(5.55072526328402,-0.433066962396004,
3.97888689800548));
#20112=CARTESIAN_POINT('Ctrl Pts',(5.57458318131544,-0.370002414621403,
3.77396688259));
#20113=CARTESIAN_POINT('Ctrl Pts',(5.59844109934686,-0.21646219781534,3.62431812139094));
#20114=CARTESIAN_POINT('Ctrl Pts',(5.62229901737828,-0.00999107731853999,
3.56653381289738));
#20115=CARTESIAN_POINT('Ctrl Pts',(5.64615693540971,0.198923133709572,3.61474379450078));
#20116=CARTESIAN_POINT('Ctrl Pts',(5.67001485344111,0.359195220034686,3.75715941257656));
#20117=CARTESIAN_POINT('Ctrl Pts',(5.69387277147254,0.431634290692432,3.95895616900985));
#20118=CARTESIAN_POINT('Ctrl Pts',(5.71773068950395,0.398527019959163,4.1707892603438));
#20119=CARTESIAN_POINT('Ctrl Pts',(5.74158860753538,0.267969036875697,4.34085972491723));
#20120=CARTESIAN_POINT('Ctrl Pts',(5.76014482567452,0.115458993192439,4.40830959117706));
#20121=CARTESIAN_POINT('Ctrl Pts',(5.77074840446986,0.0231018550196917,
4.41587281831976));
#20122=CARTESIAN_POINT('Ctrl Pts',(5.7733993439214,9.17748676073846E-6,
4.4158542849441));
#20123=CARTESIAN_POINT('Origin',(3.42660065607856,0.,4.));
#20124=CARTESIAN_POINT('',(5.07660065607859,8.10857529294212E-6,4.41589722116852));
#20125=CARTESIAN_POINT('',(5.1733993439214,1.02299162792543E-5,4.4158851107878));
#20126=CARTESIAN_POINT('',(3.42660065607856,4.87367679877478E-13,4.415875));
#20127=CARTESIAN_POINT('Ctrl Pts',(5.07660065607858,8.10857529294148E-6,
4.41589722116852));
#20128=CARTESIAN_POINT('Ctrl Pts',(5.08355518053415,-0.060555656273516,
4.41584370653314));
#20129=CARTESIAN_POINT('Ctrl Pts',(5.09846234433351,-0.190424342306974,
4.38715451669839));
#20130=CARTESIAN_POINT('Ctrl Pts',(5.1213221474767,-0.349282119693095,4.256894448863));
#20131=CARTESIAN_POINT('Ctrl Pts',(5.1451800655081,-0.4296670234643,4.05812921762123));
#20132=CARTESIAN_POINT('Ctrl Pts',(5.16903798353954,-0.404986636103755,
3.84514980926298));
#20133=CARTESIAN_POINT('Ctrl Pts',(5.19289590157095,-0.281275984601366,
3.67003549057442));
#20134=CARTESIAN_POINT('Ctrl Pts',(5.21675381960238,-0.0887856930599551,
3.5756064824932));
#20135=CARTESIAN_POINT('Ctrl Pts',(5.24061173763379,0.125415118908336,3.58495324968971));
#20136=CARTESIAN_POINT('Ctrl Pts',(5.26446965566521,0.308948518064291,3.69579025298356));
#20137=CARTESIAN_POINT('Ctrl Pts',(5.28832757369662,0.416935588964862,3.88101482593007));
#20138=CARTESIAN_POINT('Ctrl Pts',(5.31218549172805,0.422970551266107,4.09533451502773));
#20139=CARTESIAN_POINT('Ctrl Pts',(5.33604340975946,0.325577692296299,4.28634231834109));
#20140=CARTESIAN_POINT('Ctrl Pts',(5.35751513120965,0.166275769440666,4.39523064161658));
#20141=CARTESIAN_POINT('Ctrl Pts',(5.37103421331602,0.0484777907299229,
4.41581629730449));
#20142=CARTESIAN_POINT('Ctrl Pts',(5.37660065607859,-1.01751121954468E-5,
4.41586038335289));
#20143=CARTESIAN_POINT('Ctrl Pts',(5.1733993439214,1.02299162792474E-5,
4.4158851107878));
#20144=CARTESIAN_POINT('Ctrl Pts',(5.17988506021851,-0.0564756498766958,
4.41582730150705));
#20145=CARTESIAN_POINT('Ctrl Pts',(5.19432341585943,-0.182274442988225,
4.39002065289559));
#20146=CARTESIAN_POINT('Ctrl Pts',(5.21671441084416,-0.341564590845109,
4.26707000444592));
#20147=CARTESIAN_POINT('Ctrl Pts',(5.24057232887557,-0.427768622694993,
4.07075847957352));
#20148=CARTESIAN_POINT('Ctrl Pts',(5.264430246907,-0.409371574112622,3.85714457902312));
#20149=CARTESIAN_POINT('Ctrl Pts',(5.2882881649384,-0.290872024601924,3.6784627202051));
#20150=CARTESIAN_POINT('Ctrl Pts',(5.31214608296984,-0.101246341881189,
3.57840548479658));
#20151=CARTESIAN_POINT('Ctrl Pts',(5.33600400100125,0.113136829324483,3.58143959235932));
#20152=CARTESIAN_POINT('Ctrl Pts',(5.35986191903268,0.299854963974951,3.68682312094679));
#20153=CARTESIAN_POINT('Ctrl Pts',(5.38371983706408,0.413250392048343,3.8687869272297));
#20154=CARTESIAN_POINT('Ctrl Pts',(5.40757775509551,0.425594842551202,4.08283590397723));
#20155=CARTESIAN_POINT('Ctrl Pts',(5.43143567312693,0.333869761079625,4.27662924579771));
#20156=CARTESIAN_POINT('Ctrl Pts',(5.45337620273556,0.174437273907163,4.39264091290779));
#20157=CARTESIAN_POINT('Ctrl Pts',(5.46736409300038,0.0525562895569378,
4.41581883033293));
#20158=CARTESIAN_POINT('Ctrl Pts',(5.4733993439214,-1.0901499259525E-5,
4.41587264340464));
#20159=CARTESIAN_POINT('Origin',(3.42660065607856,0.,4.));
#20160=CARTESIAN_POINT('',(4.77660065607858,-3.27394476109793E-6,4.41584059078716));
#20161=CARTESIAN_POINT('',(4.8733993439214,-6.67049670156904E-6,4.4158459349409));
#20162=CARTESIAN_POINT('',(3.42660065607856,4.87367679877478E-13,4.415875));
#20163=CARTESIAN_POINT('Ctrl Pts',(4.77660065607858,-3.27394476113199E-6,
4.41584059078717));
#20164=CARTESIAN_POINT('Ctrl Pts',(4.78017086906467,-0.0311067951354469,
4.4158491206715));
#20165=CARTESIAN_POINT('Ctrl Pts',(4.79169372139456,-0.131487321212171,
4.40473555835468));
#20166=CARTESIAN_POINT('Ctrl Pts',(4.81116921306824,-0.287199161490599,
4.32482210305491));
#20167=CARTESIAN_POINT('Ctrl Pts',(4.83502713109967,-0.407721671464292,
4.14749845969467));
#20168=CARTESIAN_POINT('Ctrl Pts',(4.85888504913109,-0.42854512664958,3.93410742516172));
#20169=CARTESIAN_POINT('Ctrl Pts',(4.8827429671625,-0.344577625034195,3.73682892005441));
#20170=CARTESIAN_POINT('Ctrl Pts',(4.90660088519393,-0.176351507991885,
3.60390291263011));
#20171=CARTESIAN_POINT('Ctrl Pts',(4.93045880322534,0.0349973564730633,
3.56783343253575));
#20172=CARTESIAN_POINT('Ctrl Pts',(4.95431672125677,0.237788413971502,3.63744045016736));
#20173=CARTESIAN_POINT('Ctrl Pts',(4.97817463928818,0.382433727027559,3.79570315365689));
#20174=CARTESIAN_POINT('Ctrl Pts',(5.0020325573196,0.433563576539811,4.00392200101168));
#20175=CARTESIAN_POINT('Ctrl Pts',(5.02589047535102,0.378675321553375,4.21118181228595));
#20176=CARTESIAN_POINT('Ctrl Pts',(5.04974839338244,0.231190635538481,4.36680191797922));
#20177=CARTESIAN_POINT('Ctrl Pts',(5.0666517869583,0.086644022961884,4.4135113916189));
#20178=CARTESIAN_POINT('Ctrl Pts',(5.07560254119034,0.00870023350343714,
4.41590490160082));
#20179=CARTESIAN_POINT('Ctrl Pts',(5.07660065607858,8.10857529294148E-6,
4.41589722116852));
#20180=CARTESIAN_POINT('Ctrl Pts',(4.8733993439214,-6.67049670157252E-6,
4.41584593494091));
#20181=CARTESIAN_POINT('Ctrl Pts',(4.87650074874903,-0.0270249643080214,
4.41586127519519));
#20182=CARTESIAN_POINT('Ctrl Pts',(4.88755479292047,-0.123313358466266,
4.40662010077424));
#20183=CARTESIAN_POINT('Ctrl Pts',(4.90656147643571,-0.277507970732168,
4.33313973520738));
#20184=CARTESIAN_POINT('Ctrl Pts',(4.93041939446713,-0.403200703213916,
4.15944262266324));
#20185=CARTESIAN_POINT('Ctrl Pts',(4.95427731249855,-0.430299880793222,
3.94675744574809));
#20186=CARTESIAN_POINT('Ctrl Pts',(4.97813523052996,-0.352179016385168,
3.7470915236456));
#20187=CARTESIAN_POINT('Ctrl Pts',(5.00199314856139,-0.187940789307144,
3.60926861310034));
#20188=CARTESIAN_POINT('Ctrl Pts',(5.0258510665928,0.0222540801607904,3.56699016996131));
#20189=CARTESIAN_POINT('Ctrl Pts',(5.04970898462423,0.227007220840439,3.63059442521772));
#20190=CARTESIAN_POINT('Ctrl Pts',(5.07356690265564,0.376250912472057,3.7845284059142));
#20191=CARTESIAN_POINT('Ctrl Pts',(5.09742482068706,0.433491007135177,3.99115106069306));
#20192=CARTESIAN_POINT('Ctrl Pts',(5.12128273871848,0.384730742495793,4.19993752217271));
#20193=CARTESIAN_POINT('Ctrl Pts',(5.1451406567499,0.241893331461176,4.35983381329239));
#20194=CARTESIAN_POINT('Ctrl Pts',(5.16251285848421,0.0948160588051851,
4.41219316122439));
#20195=CARTESIAN_POINT('Ctrl Pts',(5.17193242087471,0.0127860645481494,
4.41589818594594));
#20196=CARTESIAN_POINT('Ctrl Pts',(5.1733993439214,1.02299162792474E-5,
4.4158851107878));
#20197=CARTESIAN_POINT('Origin',(3.42660065607856,0.,4.));
#20198=CARTESIAN_POINT('',(4.47660065607858,-1.72413508574122E-6,4.41591032029986));
#20199=CARTESIAN_POINT('',(4.5733993439214,2.6062779713001E-6,4.4159095790646));
#20200=CARTESIAN_POINT('',(3.42660065607856,4.87367679877478E-13,4.415875));
#20201=CARTESIAN_POINT('Ctrl Pts',(4.47660065607858,-1.72413508575881E-6,
4.41591032029986));
#20202=CARTESIAN_POINT('Ctrl Pts',(4.47678655759518,-0.00162050728124812,
4.41591069657345));
#20203=CARTESIAN_POINT('Ctrl Pts',(4.48492509845559,-0.0724886630755744,
4.4155056303295));
#20204=CARTESIAN_POINT('Ctrl Pts',(4.5010162786598,-0.212178818846594,4.37811758201071));
#20205=CARTESIAN_POINT('Ctrl Pts',(4.52487419669122,-0.367409789343613,
4.23022337776645));
#20206=CARTESIAN_POINT('Ctrl Pts',(4.54873211472264,-0.432799058467291,
4.02603328640456));
#20207=CARTESIAN_POINT('Ctrl Pts',(4.57259003275406,-0.392357168499796,
3.8154773474345));
#20208=CARTESIAN_POINT('Ctrl Pts',(4.59644795078547,-0.255973263285106,
3.65004222328625));
#20209=CARTESIAN_POINT('Ctrl Pts',(4.6203058688169,-0.0569969226013119,
3.57018130821703));
#20210=CARTESIAN_POINT('Ctrl Pts',(4.64416378684831,0.155916718210686,3.59542277130738));
#20211=CARTESIAN_POINT('Ctrl Pts',(4.66802170487973,0.330704474340828,3.71959438727947));
#20212=CARTESIAN_POINT('Ctrl Pts',(4.69187962291115,0.424625978282027,3.91233281365517));
#20213=CARTESIAN_POINT('Ctrl Pts',(4.71573754094257,0.41471486395576,4.1265082550995));
#20214=CARTESIAN_POINT('Ctrl Pts',(4.73959545897399,0.303394668785218,4.30974898215573));
#20215=CARTESIAN_POINT('Ctrl Pts',(4.75988316401932,0.145646585585232,4.40116103141851));
#20216=CARTESIAN_POINT('Ctrl Pts',(4.77221822972086,0.0381762104768988,
4.41583012037823));
#20217=CARTESIAN_POINT('Ctrl Pts',(4.77660065607858,-3.27394476113199E-6,
4.41584059078717));
#20218=CARTESIAN_POINT('Ctrl Pts',(4.5733993439214,2.60627797130011E-6,
4.4159095790646));
#20219=CARTESIAN_POINT('Ctrl Pts',(4.58106907662335,-0.0667838229435618,
4.4158868274511));
#20220=CARTESIAN_POINT('Ctrl Pts',(4.59669144866912,-0.202842099803805,
4.38250385602613));
#20221=CARTESIAN_POINT('Ctrl Pts',(4.62026646005868,-0.360469908510665,
4.24094439618412));
#20222=CARTESIAN_POINT('Ctrl Pts',(4.6441243780901,-0.431844582779732,4.03876871570463));
#20223=CARTESIAN_POINT('Ctrl Pts',(4.66798229612152,-0.397621493350665,
3.82711302819544));
#20224=CARTESIAN_POINT('Ctrl Pts',(4.69184021415294,-0.266169117804412,
3.65773291463971));
#20225=CARTESIAN_POINT('Ctrl Pts',(4.71569813218436,-0.0696311426542753,
3.57204642662242));
#20226=CARTESIAN_POINT('Ctrl Pts',(4.73955605021577,0.143933543589337,3.59100624451743));
#20227=CARTESIAN_POINT('Ctrl Pts',(4.76341396824719,0.322302557754209,3.70997617639404));
#20228=CARTESIAN_POINT('Ctrl Pts',(4.78727188627862,0.421859817202848,3.8998648332327));
#20229=CARTESIAN_POINT('Ctrl Pts',(4.81112980431003,0.41826086011465,4.11423926597311));
#20230=CARTESIAN_POINT('Ctrl Pts',(4.83498772234146,0.312385729531365,4.30067908636799));
#20231=CARTESIAN_POINT('Ctrl Pts',(4.85574423554524,0.15381688120809,4.39891624198015));
#20232=CARTESIAN_POINT('Ctrl Pts',(4.86854810940522,0.04225549351942,4.41582193963064));
#20233=CARTESIAN_POINT('Ctrl Pts',(4.8733993439214,-6.67049670157252E-6,
4.41584593494091));
#20234=CARTESIAN_POINT('Origin',(3.42660065607856,0.,4.));
#20235=CARTESIAN_POINT('',(4.17660065607858,5.88453344125852E-6,4.41584444980552));
#20236=CARTESIAN_POINT('',(4.2733993439214,2.51014653358805E-6,4.41583996132385));
#20237=CARTESIAN_POINT('',(3.42660065607856,4.87367679877478E-13,4.415875));
#20238=CARTESIAN_POINT('Ctrl Pts',(4.17660065607858,5.88453344126799E-6,
4.41584444980552));
#20239=CARTESIAN_POINT('Ctrl Pts',(4.18135488546951,-0.0414115481342504,
4.41582334930757));
#20240=CARTESIAN_POINT('Ctrl Pts',(4.19406175420423,-0.152126265423154,
4.3993918905015));
#20241=CARTESIAN_POINT('Ctrl Pts',(4.21472126228278,-0.310547447266788,
4.30257739619942));
#20242=CARTESIAN_POINT('Ctrl Pts',(4.23857918031418,-0.417556725585918,
4.11678647978038));
#20243=CARTESIAN_POINT('Ctrl Pts',(4.26243709834561,-0.422462345057068,
3.90243789311793));
#20244=CARTESIAN_POINT('Ctrl Pts',(4.28629501637703,-0.324064236326554,
3.71194600226016));
#20245=CARTESIAN_POINT('Ctrl Pts',(4.31015293440845,-0.146423688323203,
3.59189110566319));
#20246=CARTESIAN_POINT('Ctrl Pts',(4.33401085243986,0.0670214896752265,
3.5716299793216));
#20247=CARTESIAN_POINT('Ctrl Pts',(4.35786877047129,0.264078061498623,3.65611697628114));
#20248=CARTESIAN_POINT('Ctrl Pts',(4.38172668850271,0.396560367883193,3.82469274783887));
#20249=CARTESIAN_POINT('Ctrl Pts',(4.40558460653412,0.432072854850341,4.03613591352675));
#20250=CARTESIAN_POINT('Ctrl Pts',(4.42944252456555,0.361931763288092,4.23874286631049));
#20251=CARTESIAN_POINT('Ctrl Pts',(4.45311454108036,0.204524647174786,4.38184685695289));
#20252=CARTESIAN_POINT('Ctrl Pts',(4.46883391825138,0.0676290543833733,
4.4158946000499));
#20253=CARTESIAN_POINT('Ctrl Pts',(4.47660065607858,-1.72413508575881E-6,
4.41591032029986));
#20254=CARTESIAN_POINT('Ctrl Pts',(4.2733993439214,2.51014653359152E-6,
4.41583996132385));
#20255=CARTESIAN_POINT('Ctrl Pts',(4.27768476515387,-0.0373320337329404,
4.41583213221101));
#20256=CARTESIAN_POINT('Ctrl Pts',(4.28992282573015,-0.143955736965383,
4.40160880992953));
#20257=CARTESIAN_POINT('Ctrl Pts',(4.31011352565024,-0.301501118270308,
4.3115924136571));
#20258=CARTESIAN_POINT('Ctrl Pts',(4.33397144368164,-0.413936097932681,
4.12903358037428));
#20259=CARTESIAN_POINT('Ctrl Pts',(4.35782936171308,-0.425152419412173,
3.91492252699502));
#20260=CARTESIAN_POINT('Ctrl Pts',(4.38168727974448,-0.332407397051365,
3.72161523052345));
#20261=CARTESIAN_POINT('Ctrl Pts',(4.40554519777592,-0.158379709595794,
3.5963805946708));
#20262=CARTESIAN_POINT('Ctrl Pts',(4.42940311580732,0.0543761300157755,
3.56984189703405));
#20263=CARTESIAN_POINT('Ctrl Pts',(4.45326103383876,0.25383552520097,3.64848857324589));
#20264=CARTESIAN_POINT('Ctrl Pts',(4.47711895187016,0.39122521984844,3.81308936806525));
#20265=CARTESIAN_POINT('Ctrl Pts',(4.50097686990159,0.432949691632991,4.02339490384879));
#20266=CARTESIAN_POINT('Ctrl Pts',(4.524834787933,0.368806170420464,4.22797974831721));
#20267=CARTESIAN_POINT('Ctrl Pts',(4.54869270596443,0.214479494504121,4.37681733431002));
#20268=CARTESIAN_POINT('Ctrl Pts',(4.56488089129389,0.0741790848482271,
4.4152866170047));
#20269=CARTESIAN_POINT('Ctrl Pts',(4.57311643727954,0.0024660981813593,
4.41591041828323));
#20270=CARTESIAN_POINT('Ctrl Pts',(4.5733993439214,2.60627797130011E-6,
4.4159095790646));
#20271=CARTESIAN_POINT('Ctrl Pts',(3.95224475517895,0.178288362465424,4.37571967666652));
#20272=CARTESIAN_POINT('Ctrl Pts',(3.96019739452275,0.115708609995841,4.40541533085819));
#20273=CARTESIAN_POINT('Ctrl Pts',(3.97610267321037,-0.0245105356436035,
4.43290545314371));
#20274=CARTESIAN_POINT('Ctrl Pts',(3.99996059124178,-0.228962993402626,
4.36819499612132));
#20275=CARTESIAN_POINT('Ctrl Pts',(4.0238185092732,-0.377374743411151,4.21349068386271));
#20276=CARTESIAN_POINT('Ctrl Pts',(4.04767642730463,-0.433534992178268,
4.00656196868444));
#20277=CARTESIAN_POINT('Ctrl Pts',(4.07153434533603,-0.383670022685343,
3.79803920418254));
#20278=CARTESIAN_POINT('Ctrl Pts',(4.09539226336747,-0.239994733226421,
3.63889579340969));
#20279=CARTESIAN_POINT('Ctrl Pts',(4.11925018139887,-0.0376302499649443,
3.56805514133307));
#20280=CARTESIAN_POINT('Ctrl Pts',(4.1431080994303,0.173933765839147,3.60283521426327));
#20281=CARTESIAN_POINT('Ctrl Pts',(4.16696601746172,0.342967344134064,3.73473372141871));
#20282=CARTESIAN_POINT('Ctrl Pts',(4.19082393549313,0.428135478754777,3.93149662217858));
#20283=CARTESIAN_POINT('Ctrl Pts',(4.21468185352456,0.40861313688017,4.1450106963618));
#20284=CARTESIAN_POINT('Ctrl Pts',(4.23853977155597,0.289173588337559,4.32306558264197));
#20285=CARTESIAN_POINT('Ctrl Pts',(4.2623976895874,0.0990233075312312,4.42212219878201));
#20286=CARTESIAN_POINT('Ctrl Pts',(4.28625560761881,-0.115340915390822,
4.41795840454656));
#20287=CARTESIAN_POINT('Ctrl Pts',(4.31011352565024,-0.301501118270308,
4.3115924136571));
#20288=CARTESIAN_POINT('Ctrl Pts',(4.33397144368164,-0.413936097932681,
4.12903358037428));
#20289=CARTESIAN_POINT('Ctrl Pts',(4.35782936171308,-0.425152419412173,
3.91492252699502));
#20290=CARTESIAN_POINT('Ctrl Pts',(4.38168727974448,-0.332407397051365,
3.72161523052345));
#20291=CARTESIAN_POINT('Ctrl Pts',(4.40554519777592,-0.158379709595794,
3.5963805946708));
#20292=CARTESIAN_POINT('Ctrl Pts',(4.42940311580732,0.0543761300157755,
3.56984189703405));
#20293=CARTESIAN_POINT('Ctrl Pts',(4.45326103383876,0.25383552520097,3.64848857324589));
#20294=CARTESIAN_POINT('Ctrl Pts',(4.47711895187016,0.39122521984844,3.81308936806525));
#20295=CARTESIAN_POINT('Ctrl Pts',(4.50097686990159,0.432949691632991,4.02339490384879));
#20296=CARTESIAN_POINT('Ctrl Pts',(4.524834787933,0.368806170420464,4.22797974831721));
#20297=CARTESIAN_POINT('Ctrl Pts',(4.54869270596443,0.214479494504121,4.37681733431002));
#20298=CARTESIAN_POINT('Ctrl Pts',(4.57255062399584,0.00770673985495463,
4.4335128177492));
#20299=CARTESIAN_POINT('Ctrl Pts',(4.59640854202726,-0.200950522604244,
4.38420260860549));
#20300=CARTESIAN_POINT('Ctrl Pts',(4.62026646005868,-0.360469908510665,
4.24094439618412));
#20301=CARTESIAN_POINT('Ctrl Pts',(4.6441243780901,-0.431844582779732,4.03876871570463));
#20302=CARTESIAN_POINT('Ctrl Pts',(4.66798229612152,-0.397621493350665,
3.82711302819544));
#20303=CARTESIAN_POINT('Ctrl Pts',(4.69184021415294,-0.266169117804412,
3.65773291463971));
#20304=CARTESIAN_POINT('Ctrl Pts',(4.71569813218436,-0.0696311426542753,
3.57204642662242));
#20305=CARTESIAN_POINT('Ctrl Pts',(4.73955605021577,0.143933543589337,3.59100624451743));
#20306=CARTESIAN_POINT('Ctrl Pts',(4.76341396824719,0.322302557754209,3.70997617639404));
#20307=CARTESIAN_POINT('Ctrl Pts',(4.78727188627862,0.421859817202848,3.8998648332327));
#20308=CARTESIAN_POINT('Ctrl Pts',(4.81112980431003,0.41826086011465,4.11423926597311));
#20309=CARTESIAN_POINT('Ctrl Pts',(4.83498772234146,0.312385729531365,4.30067908636799));
#20310=CARTESIAN_POINT('Ctrl Pts',(4.85884564037287,0.130123778861223,4.41359467981201));
#20311=CARTESIAN_POINT('Ctrl Pts',(4.88270355840429,-0.0839569802410516,
4.42537510794913));
#20312=CARTESIAN_POINT('Ctrl Pts',(4.90656147643571,-0.277507970732168,
4.33313973520738));
#20313=CARTESIAN_POINT('Ctrl Pts',(4.93041939446713,-0.403200703213916,
4.15944262266324));
#20314=CARTESIAN_POINT('Ctrl Pts',(4.95427731249855,-0.430299880793222,
3.94675744574809));
#20315=CARTESIAN_POINT('Ctrl Pts',(4.97813523052996,-0.352179016385168,
3.7470915236456));
#20316=CARTESIAN_POINT('Ctrl Pts',(5.00199314856139,-0.187940789307144,
3.60926861310034));
#20317=CARTESIAN_POINT('Ctrl Pts',(5.0258510665928,0.0222540801607904,3.56699016996131));
#20318=CARTESIAN_POINT('Ctrl Pts',(5.04970898462423,0.227007220840439,3.63059442521772));
#20319=CARTESIAN_POINT('Ctrl Pts',(5.07356690265564,0.376250912472057,3.7845284059142));
#20320=CARTESIAN_POINT('Ctrl Pts',(5.09742482068706,0.433491007135177,3.99115106069306));
#20321=CARTESIAN_POINT('Ctrl Pts',(5.12128273871848,0.384730742495793,4.19993752217271));
#20322=CARTESIAN_POINT('Ctrl Pts',(5.1451406567499,0.241893331461176,4.35983381329239));
#20323=CARTESIAN_POINT('Ctrl Pts',(5.16899857478132,0.0399064118422473,
4.43174093538579));
#20324=CARTESIAN_POINT('Ctrl Pts',(5.19285649281273,-0.171838712500945,
4.39807563839043));
#20325=CARTESIAN_POINT('Ctrl Pts',(5.21671441084416,-0.341564590845109,
4.26707000444592));
#20326=CARTESIAN_POINT('Ctrl Pts',(5.24057232887557,-0.427768622694993,
4.07075847957352));
#20327=CARTESIAN_POINT('Ctrl Pts',(5.264430246907,-0.409371574112622,3.85714457902312));
#20328=CARTESIAN_POINT('Ctrl Pts',(5.2882881649384,-0.290872024601924,3.6784627202051));
#20329=CARTESIAN_POINT('Ctrl Pts',(5.31214608296984,-0.101246341881189,
3.57840548479658));
#20330=CARTESIAN_POINT('Ctrl Pts',(5.33600400100125,0.113136829324483,3.58143959235932));
#20331=CARTESIAN_POINT('Ctrl Pts',(5.35986191903268,0.299854963974951,3.68682312094679));
#20332=CARTESIAN_POINT('Ctrl Pts',(5.38371983706408,0.413250392048343,3.8687869272297));
#20333=CARTESIAN_POINT('Ctrl Pts',(5.40757775509551,0.425594842551202,4.08283590397723));
#20334=CARTESIAN_POINT('Ctrl Pts',(5.43143567312693,0.333869761079625,4.27662924579771));
#20335=CARTESIAN_POINT('Ctrl Pts',(5.45529359115834,0.160504428594232,4.4027792017911));
#20336=CARTESIAN_POINT('Ctrl Pts',(5.47915150918977,-0.0521086087350157,
4.43043867146175));
#20337=CARTESIAN_POINT('Ctrl Pts',(5.50300942722118,-0.251979671819092,
4.35284416104532));
#20338=CARTESIAN_POINT('Ctrl Pts',(5.52686734525261,-0.390234841353927,
4.18896964197264));
#20339=CARTESIAN_POINT('Ctrl Pts',(5.55072526328402,-0.433066962396004,
3.97888689800548));
#20340=CARTESIAN_POINT('Ctrl Pts',(5.57458318131544,-0.370002414621403,
3.77396688259));
#20341=CARTESIAN_POINT('Ctrl Pts',(5.59844109934686,-0.21646219781534,3.62431812139094));
#20342=CARTESIAN_POINT('Ctrl Pts',(5.62229901737828,-0.00999107731853999,
3.56653381289738));
#20343=CARTESIAN_POINT('Ctrl Pts',(5.64615693540971,0.198923133709572,3.61474379450078));
#20344=CARTESIAN_POINT('Ctrl Pts',(5.67001485344111,0.359195220034686,3.75715941257656));
#20345=CARTESIAN_POINT('Ctrl Pts',(5.69387277147254,0.431634290692432,3.95895616900985));
#20346=CARTESIAN_POINT('Ctrl Pts',(5.71773068950395,0.398527019959163,4.1707892603438));
#20347=CARTESIAN_POINT('Ctrl Pts',(5.74158860753538,0.267969036875697,4.34085972491723));
#20348=CARTESIAN_POINT('Ctrl Pts',(5.76544652556679,0.0718853255354575,
4.42758070267197));
#20349=CARTESIAN_POINT('Ctrl Pts',(5.78930444359821,-0.141776307127955,
4.40974655013133));
#20350=CARTESIAN_POINT('Ctrl Pts',(5.81316236162963,-0.320769768688322,
4.29171820750724));
#20351=CARTESIAN_POINT('Ctrl Pts',(5.83702027966105,-0.421326288178809,
4.10235681181338));
#20352=CARTESIAN_POINT('Ctrl Pts',(5.86087819769247,-0.418857046020503,
3.88796639709818));
#20353=CARTESIAN_POINT('Ctrl Pts',(5.88473611572389,-0.313965860818636,
3.70097123187977));
#20354=CARTESIAN_POINT('Ctrl Pts',(5.90859403375531,-0.132301443679057,
3.58709678011166));
#20355=CARTESIAN_POINT('Ctrl Pts',(5.93245195178673,0.0817142298265842,
3.57418834816524));
#20356=CARTESIAN_POINT('Ctrl Pts',(5.95630986981814,0.275748643515392,3.66540258613358));
#20357=CARTESIAN_POINT('Ctrl Pts',(5.98016778784957,0.402354822815078,3.83843477537114));
#20358=CARTESIAN_POINT('Ctrl Pts',(6.00402570588098,0.430574627524036,4.05097449853386));
#20359=CARTESIAN_POINT('Ctrl Pts',(6.02788362391241,0.353506566116634,4.25104874587108));
#20360=CARTESIAN_POINT('Ctrl Pts',(6.05174154194382,0.189997730437525,4.38973628930191));
#20361=CARTESIAN_POINT('Ctrl Pts',(6.07559945997525,-0.0199730113800777,
4.43311976162365));
#20362=CARTESIAN_POINT('Ctrl Pts',(6.09945737800665,-0.2250554921608,4.3705991908187));
#20363=CARTESIAN_POINT('Ctrl Pts',(6.12331529603809,-0.375113923638194,
4.21744656883549));
#20364=CARTESIAN_POINT('Ctrl Pts',(6.1471732140695,-0.433431396087355,4.01114207710762));
#20365=CARTESIAN_POINT('Ctrl Pts',(6.17103113210093,-0.385792139046387,
3.80207577201042));
#20366=CARTESIAN_POINT('Ctrl Pts',(6.19488905013233,-0.243761337718234,
3.64147770828707));
#20367=CARTESIAN_POINT('Ctrl Pts',(6.21874696816376,-0.042227823444436,
3.56841523311022));
#20368=CARTESIAN_POINT('Ctrl Pts',(6.24260488619517,0.16982704650124,3.60113783246665));
#20369=CARTESIAN_POINT('Ctrl Pts',(6.2664628042266,0.339985970990829,3.73091992247201));
#20370=CARTESIAN_POINT('Ctrl Pts',(6.29032072225801,0.427700638223926,3.92738904240251));
#20371=CARTESIAN_POINT('Ctrl Pts',(6.31417864028943,0.409561128158778,4.13996490148311));
#20372=CARTESIAN_POINT('Ctrl Pts',(6.34598919766466,0.254661277208374,4.38159318714805));
#20373=CARTESIAN_POINT('Ctrl Pts',(6.38575239438369,-0.125272905304917,
4.47558432627151));
#20374=CARTESIAN_POINT('Ctrl Pts',(6.43346823044653,-0.468271923807345,
4.15124960425567));
#20375=CARTESIAN_POINT('Ctrl Pts',(6.48118406650937,-0.380227249479543,
3.6882349865083));
#20376=CARTESIAN_POINT('Ctrl Pts',(6.52889990257221,0.0564566449812287,
3.51140415777354));
#20377=CARTESIAN_POINT('Ctrl Pts',(6.57661573863504,0.441574375138847,3.78331933667001));
#20378=CARTESIAN_POINT('Ctrl Pts',(6.62433157469789,0.421040068198854,4.25418342072721));
#20379=CARTESIAN_POINT('Ctrl Pts',(6.67204741076071,0.0139362792425842,
4.49164405688148));
#20380=CARTESIAN_POINT('Ctrl Pts',(6.71976324682356,-0.406006764042365,
4.27761133505345));
#20381=CARTESIAN_POINT('Ctrl Pts',(6.76747908288639,-0.453085647428837,
3.80864864857145));
#20382=CARTESIAN_POINT('Ctrl Pts',(6.81519491894923,-0.0841006081168706,
3.51540431248109));
#20383=CARTESIAN_POINT('Ctrl Pts',(6.86291075501207,0.362121456530253,3.66717299786736));
#20384=CARTESIAN_POINT('Ctrl Pts',(6.91062659107491,0.475798562415156,4.124581128109));
#20385=CARTESIAN_POINT('Ctrl Pts',(6.95834242713775,0.152544250279933,4.46758486877347));
#20386=CARTESIAN_POINT('Ctrl Pts',(7.00605826320058,-0.310794706562241,
4.38119802990972));
#20387=CARTESIAN_POINT('Ctrl Pts',(7.05377409926342,-0.488725618924084,
3.94475128051735));
#20388=CARTESIAN_POINT('Ctrl Pts',(7.10148993532626,-0.21785253135038,3.55904022429238));
#20389=CARTESIAN_POINT('Ctrl Pts',(7.14920577138909,0.253078023397415,3.57826934481931));
#20390=CARTESIAN_POINT('Ctrl Pts',(7.19692160745195,0.491603063369337,3.98478019943955));
#20391=CARTESIAN_POINT('Ctrl Pts',(7.24463744351477,0.278681483980911,4.40526763942622));
#20392=CARTESIAN_POINT('Ctrl Pts',(7.29235327957762,-0.190157610347023,
4.45359156587464));
#20393=CARTESIAN_POINT('Ctrl Pts',(7.34006911564044,-0.484372034479295,
4.08537538031203));
#20394=CARTESIAN_POINT('Ctrl Pts',(7.3877849517033,-0.333780171974684,3.63875766810317));
#20395=CARTESIAN_POINT('Ctrl Pts',(7.43550078776612,0.123327161313159,3.52387434835784));
#20396=CARTESIAN_POINT('Ctrl Pts',(7.48321662382897,0.467181263150904,3.84622454030349));
#20397=CARTESIAN_POINT('Ctrl Pts',(7.5309324598918,0.382015623368301,4.30978910321172));
#20398=CARTESIAN_POINT('Ctrl Pts',(7.57864829595465,-0.0539608418635878,
4.4888695658253));
#20399=CARTESIAN_POINT('Ctrl Pts',(7.62636413201748,-0.440384235482588,
4.21901358396786));
#20400=CARTESIAN_POINT('Ctrl Pts',(7.67407996808031,-0.422396009600076,
3.7480340579683));
#20401=CARTESIAN_POINT('Ctrl Pts',(7.72179580414317,-0.0165150286377962,
3.50843873354525));
#20402=CARTESIAN_POINT('Ctrl Pts',(7.76951164020598,0.404531957204003,3.72025168374225));
#20403=CARTESIAN_POINT('Ctrl Pts',(7.81722747626884,0.454091022239626,4.18896181724392));
#20404=CARTESIAN_POINT('Ctrl Pts',(7.86494331233166,0.0866513144543145,
4.48414540641706));
#20405=CARTESIAN_POINT('Ctrl Pts',(7.91265914839452,-0.360361628691054,
4.33473081934393));
#20406=CARTESIAN_POINT('Ctrl Pts',(7.96037498445733,-0.476448943335793,
3.87792777037096));
#20407=CARTESIAN_POINT('Ctrl Pts',(8.0080908205202,-0.1550058622045,3.53322552818936));
#20408=CARTESIAN_POINT('Ctrl Pts',(8.05580665658301,0.308781487260178,3.61716946571973));
#20409=CARTESIAN_POINT('Ctrl Pts',(8.10352249264587,0.489010045760349,4.0526725734847));
#20410=CARTESIAN_POINT('Ctrl Pts',(8.1512383287087,0.220173154851853,4.43980564654689));
#20411=CARTESIAN_POINT('Ctrl Pts',(8.19895416477154,-0.250852131956433,
4.4230584271054));
#20412=CARTESIAN_POINT('Ctrl Pts',(8.24667000083438,-0.491516046133,4.01781014446235));
#20413=CARTESIAN_POINT('Ctrl Pts',(8.29438583689722,-0.280813212199106,
3.59620653211525));
#20414=CARTESIAN_POINT('Ctrl Pts',(8.34210167296004,0.187764715363875,3.54541267448783));
#20415=CARTESIAN_POINT('Ctrl Pts',(8.38981750902289,0.483915415676709,3.91207335260334));
#20416=CARTESIAN_POINT('Ctrl Pts',(8.43753334508573,0.335679143777854,4.35947842394856));
#20417=CARTESIAN_POINT('Ctrl Pts',(8.48524918114857,-0.120816450939738,
4.4767689272953));
#20418=CARTESIAN_POINT('Ctrl Pts',(8.5329650172114,-0.466364439759318,4.15623518867385));
#20419=CARTESIAN_POINT('Ctrl Pts',(8.58068085327425,-0.383642787608637,
3.69222827230584));
#20420=CARTESIAN_POINT('Ctrl Pts',(8.62839668933707,0.0513839395061145,
3.51085286915611));
#20421=CARTESIAN_POINT('Ctrl Pts',(8.67611252539993,0.439224004328866,3.77866880275638));
#20422=CARTESIAN_POINT('Ctrl Pts',(8.72382836146275,0.42371790764641,4.24973658040369));
#20423=CARTESIAN_POINT('Ctrl Pts',(8.7715441975256,0.0191051366342138,4.49146741357506));
#20424=CARTESIAN_POINT('Ctrl Pts',(8.81926003358843,-0.403052175319494,
4.28187615866228));
#20425=CARTESIAN_POINT('Ctrl Pts',(8.86697586965126,-0.455080472922433,
3.81343369002772));
#20426=CARTESIAN_POINT('Ctrl Pts',(8.91469170571412,-0.0892013699275644,
3.51631793453238));
#20427=CARTESIAN_POINT('Ctrl Pts',(8.96240754177693,0.358592723611288,3.66337486216116));
#20428=CARTESIAN_POINT('Ctrl Pts',(9.0101233778398,0.477085601399612,4.11955983351088));
#20429=CARTESIAN_POINT('Ctrl Pts',(9.05783921390261,0.157463430517111,4.46595117008304));
#20430=CARTESIAN_POINT('Ctrl Pts',(9.10555504996547,-0.306759831495564,
4.38445237758765));
#20431=CARTESIAN_POINT('Ctrl Pts',(9.1532708860283,-0.489280820139143,3.94990505119329));
#20432=CARTESIAN_POINT('Ctrl Pts',(9.20098672209113,-0.222487703095825,
3.56136068709803));
#20433=CARTESIAN_POINT('Ctrl Pts',(9.24870255815399,0.248619295113741,3.57562555337399));
#20434=CARTESIAN_POINT('Ctrl Pts',(9.29641839421681,0.49141536912078,3.97960000382683));
#20435=CARTESIAN_POINT('Ctrl Pts',(9.34413423027966,0.282937148266828,4.40230808465976));
#20436=CARTESIAN_POINT('Ctrl Pts',(9.39185006634249,-0.185366609388173,
4.45557046104408));
#20437=CARTESIAN_POINT('Ctrl Pts',(9.43956590240532,-0.483445357410111,
4.09047547319903));
#20438=CARTESIAN_POINT('Ctrl Pts',(9.48728173846818,-0.337568794959357,
3.64229546617122));
#20439=CARTESIAN_POINT('Ctrl Pts',(9.53499757453099,0.118302386066128,3.5226010365501));
#20440=CARTESIAN_POINT('Ctrl Pts',(9.58271341059386,0.465534665650901,3.84130942079228));
#20441=CARTESIAN_POINT('Ctrl Pts',(9.63042924665667,0.385259298596883,4.30574580568933));
#20442=CARTESIAN_POINT('Ctrl Pts',(9.67814508271952,-0.0488056103349303,
4.48941111271794));
#20443=CARTESIAN_POINT('Ctrl Pts',(9.72586091878235,-0.438051576325333,
4.22364266437974));
#20444=CARTESIAN_POINT('Ctrl Pts',(9.77357675484519,-0.425028039486299,
3.75249971615691));
#20445=CARTESIAN_POINT('Ctrl Pts',(9.82129259090803,-0.0216947140899849,
3.50864008686857));
#20446=CARTESIAN_POINT('Ctrl Pts',(9.86900842697087,0.401561201071248,3.7160038263529));
#20447=CARTESIAN_POINT('Ctrl Pts',(9.91672426303371,0.456057286475463,4.18416562194019));
#20448=CARTESIAN_POINT('Ctrl Pts',(9.96444009909655,0.0917489483659128,
4.48320529314746));
#20449=CARTESIAN_POINT('Ctrl Pts',(10.0121559351594,-0.356813860767086,
4.3385101085883));
#20450=CARTESIAN_POINT('Ctrl Pts',(10.0598717712222,-0.477709011270712,
3.88295588266498));
#20451=CARTESIAN_POINT('Ctrl Pts',(10.1075876072851,-0.159916626226494,
3.53488507064564));
#20452=CARTESIAN_POINT('Ctrl Pts',(10.1553034433479,0.304729657315094,3.61393645496551));
#20453=CARTESIAN_POINT('Ctrl Pts',(10.2030192794107,0.489538007675758,4.04751593304174));
#20454=CARTESIAN_POINT('Ctrl Pts',(10.2507351154736,0.224796073077312,4.43746079867915));
#20455=CARTESIAN_POINT('Ctrl Pts',(10.2984509515364,-0.246379554360218,
4.42567868168988));
#20456=CARTESIAN_POINT('Ctrl Pts',(10.3461667875993,-0.491301045992024,
4.02298928139638));
#20457=CARTESIAN_POINT('Ctrl Pts',(10.3938826236621,-0.285053227451061,
3.599188470261));
#20458=CARTESIAN_POINT('Ctrl Pts',(10.4415984597249,0.182963355965895,3.54345905416307));
#20459=CARTESIAN_POINT('Ctrl Pts',(10.4893142957878,0.482961874346273,3.9069782134126));
#20460=CARTESIAN_POINT('Ctrl Pts',(10.5370301318506,0.339449072190825,4.35592071060949));
#20461=CARTESIAN_POINT('Ctrl Pts',(10.5847459679134,-0.115785036052801,
4.47801574270962));
#20462=CARTESIAN_POINT('Ctrl Pts',(10.6324618039763,-0.464691964107356,
4.16114156306187));
#20463=CARTESIAN_POINT('Ctrl Pts',(10.6801776400391,-0.386865111317189,
3.69628860657276));
#20464=CARTESIAN_POINT('Ctrl Pts',(10.7278934761019,0.0462259258804368,
3.51033849586834));
#20465=CARTESIAN_POINT('Ctrl Pts',(10.7756093121648,0.436866984064762,3.77405207881873));
#20466=CARTESIAN_POINT('Ctrl Pts',(10.8233251482276,0.426326368719826,4.24525711444552));
#20467=CARTESIAN_POINT('Ctrl Pts',(10.8710409842905,0.0242836891050981,
4.49123876811122));
#20468=CARTESIAN_POINT('Ctrl Pts',(10.9187568203533,-0.400059075867425,
4.28610830234036));
#20469=CARTESIAN_POINT('Ctrl Pts',(10.9664726564161,-0.45702143577077,3.81824018018824));
#20470=CARTESIAN_POINT('Ctrl Pts',(11.014188492479,-0.0942939790271268,
3.51728489730359));
#20471=CARTESIAN_POINT('Ctrl Pts',(11.0619043285418,0.355025089556487,3.65961432075161));
#20472=CARTESIAN_POINT('Ctrl Pts',(11.1096201646047,0.478319155637209,4.11452515096033));
#20473=CARTESIAN_POINT('Ctrl Pts',(11.1573360006675,0.16236538121005,4.46426577284621));
#20474=CARTESIAN_POINT('Ctrl Pts',(11.2050518367304,-0.302691021094817,
4.38766399188028));
#20475=CARTESIAN_POINT('Ctrl Pts',(11.2527676727932,-0.489781601228288,
3.95506440219344));
#20476=CARTESIAN_POINT('Ctrl Pts',(11.300483508856,-0.227098200695192,3.56372986339542));
#20477=CARTESIAN_POINT('Ctrl Pts',(11.3481993449188,0.244132971891272,3.57302890392028));
#20478=CARTESIAN_POINT('Ctrl Pts',(11.3959151809817,0.491173079921361,3.97442207176994));
#20479=CARTESIAN_POINT('Ctrl Pts',(11.4436310170445,0.287161390990383,4.39930384468027));
#20480=CARTESIAN_POINT('Ctrl Pts',(11.4913468531074,-0.180555021833016,
4.45749875294131));
#20481=CARTESIAN_POINT('Ctrl Pts',(11.5390626891702,-0.482464979911041,
4.09556551685319));
#20482=CARTESIAN_POINT('Ctrl Pts',(11.586778525233,-0.341319923258817,3.64587299617429));
#20483=CARTESIAN_POINT('Ctrl Pts',(11.6344943612959,0.113264470804062,3.5213807520529));
#20484=CARTESIAN_POINT('Ctrl Pts',(11.6822101973587,0.463836358529674,3.83641192782507));
#20485=CARTESIAN_POINT('Ctrl Pts',(11.7299260334216,0.38846018117773,4.30166854740152));
#20486=CARTESIAN_POINT('Ctrl Pts',(11.7776418694844,-0.0436449577779122,
4.48989829813191));
#20487=CARTESIAN_POINT('Ctrl Pts',(11.8253577055472,-0.435670260442099,
4.22824690363353));
#20488=CARTESIAN_POINT('Ctrl Pts',(11.8730735416101,-0.427612859293677,
3.75699286549843));
#20489=CARTESIAN_POINT('Ctrl Pts',(11.9207893776729,-0.0268719897862959,
3.50889601812151));
#20490=CARTESIAN_POINT('Ctrl Pts',(11.9685052137357,0.398545841420554,3.71178751390968));
#20491=CARTESIAN_POINT('Ctrl Pts',(12.0162210497986,0.457972894034889,4.17934897039372));
#20492=CARTESIAN_POINT('Ctrl Pts',(12.0639368858614,0.0968363912382316,
4.48221150772657));
#20493=CARTESIAN_POINT('Ctrl Pts',(12.1116527219243,-0.353226459651896,
4.34225179773635));
#20494=CARTESIAN_POINT('Ctrl Pts',(12.1593685579871,-0.478916017555994,
3.88799699566402));
#20495=CARTESIAN_POINT('Ctrl Pts',(12.2070843940499,-0.164809627468288,
3.53659627586117));
#20496=CARTESIAN_POINT('Ctrl Pts',(12.2548002301128,0.300643979445627,3.61074632631782));
#20497=CARTESIAN_POINT('Ctrl Pts',(12.3025160661756,0.490011594032383,4.04235401475446));
#20498=CARTESIAN_POINT('Ctrl Pts',(12.3502319022385,0.229394022021679,4.43506735974179));
#20499=CARTESIAN_POINT('Ctrl Pts',(12.3979477383013,-0.241879610092261,
4.42825165390643));
#20500=CARTESIAN_POINT('Ctrl Pts',(12.4456635743641,-0.491031474462283,
4.0281658647901));
#20501=CARTESIAN_POINT('Ctrl Pts',(12.493379410427,-0.289261580343189,3.60221492864948));
#20502=CARTESIAN_POINT('Ctrl Pts',(12.5410952464898,0.178141673866572,3.54155614424011));
#20503=CARTESIAN_POINT('Ctrl Pts',(12.5888110825527,0.481954687902679,3.90189340664049));
#20504=CARTESIAN_POINT('Ctrl Pts',(12.6365269186155,0.343181296211668,4.35232346328687));
#20505=CARTESIAN_POINT('Ctrl Pts',(12.6842427546783,-0.110740760313508,
4.47920946240362));
#20506=CARTESIAN_POINT('Ctrl Pts',(12.7319585907412,-0.462967872677167,
4.16603003860975));
#20507=CARTESIAN_POINT('Ctrl Pts',(12.779674426804,-0.390044463885,3.70038267566003));
#20508=CARTESIAN_POINT('Ctrl Pts',(12.8273902628668,0.0410627776982723,
3.50987851185683));
#20509=CARTESIAN_POINT('Ctrl Pts',(12.8751060989297,0.434461438689172,3.76946045210395));
#20510=CARTESIAN_POINT('Ctrl Pts',(12.9228219349925,0.42888747548329,4.24075040649094));
#20511=CARTESIAN_POINT('Ctrl Pts',(12.9705377710553,0.0294595442590321,
4.49095555817611));
#20512=CARTESIAN_POINT('Ctrl Pts',(13.0182536071182,-0.397021539751646,
4.29030866646591));
#20513=CARTESIAN_POINT('Ctrl Pts',(13.065969443181,-0.458911634846768,3.82306685936703));
#20514=CARTESIAN_POINT('Ctrl Pts',(13.1136852792439,-0.0993761143989603,
3.51830547777773));
#20515=CARTESIAN_POINT('Ctrl Pts',(13.1614011153067,0.351418020999476,3.65589158776806));
#20516=CARTESIAN_POINT('Ctrl Pts',(13.2091169513695,0.479499580452807,4.10947774749948));
#20517=CARTESIAN_POINT('Ctrl Pts',(13.2568327874324,0.167249297126924,4.46252880717046));
#20518=CARTESIAN_POINT('Ctrl Pts',(13.3045486234952,-0.298588589211839,
4.39083254629632));
#20519=CARTESIAN_POINT('Ctrl Pts',(13.352264459558,-0.490227979701372,3.96022874442655));
#20520=CARTESIAN_POINT('Ctrl Pts',(13.3999802956209,-0.23168347330409,3.56614749850931));
#20521=CARTESIAN_POINT('Ctrl Pts',(13.4476961316837,0.239619531536799,3.57047968038978));
#20522=CARTESIAN_POINT('Ctrl Pts',(13.4954119677466,0.490876233547033,3.96924698078795));
#20523=CARTESIAN_POINT('Ctrl Pts',(13.5431278038094,0.291353737189313,4.39625525192456));
#20524=CARTESIAN_POINT('Ctrl Pts',(13.5908436398722,-0.175723379082843,
4.45937622804808));
#20525=CARTESIAN_POINT('Ctrl Pts',(13.6385594759351,-0.481431012491488,
4.10064494554323));
#20526=CARTESIAN_POINT('Ctrl Pts',(13.6862753119979,-0.345033139360895,
3.64948986092447));
#20527=CARTESIAN_POINT('Ctrl Pts',(13.7339911480608,0.108213974662067,3.52021363031051));
#20528=CARTESIAN_POINT('Ctrl Pts',(13.7817069841236,0.462086530666827,3.83153260544464));
#20529=CARTESIAN_POINT('Ctrl Pts',(13.8294228201864,0.391617915445045,4.297557781203));
#20530=CARTESIAN_POINT('Ctrl Pts',(13.8771386562493,-0.0384794573460961,
4.49033106796769));
#20531=CARTESIAN_POINT('Ctrl Pts',(13.9248544923121,-0.433240552373761,
4.23282579030437));
#20532=CARTESIAN_POINT('Ctrl Pts',(13.9725703283749,-0.430150181893835,
3.76151300691929));
#20533=CARTESIAN_POINT('Ctrl Pts',(14.0202861644378,-0.032046280669499,
3.50920649887429));
#20534=CARTESIAN_POINT('Ctrl Pts',(14.0680020005006,0.39548621318905,3.70760321474174));
#20535=CARTESIAN_POINT('Ctrl Pts',(14.1157178365634,0.459837632138507,4.1745123976147));
#20536=CARTESIAN_POINT('Ctrl Pts',(14.1634336726263,0.101913077983734,4.48116416053968));
#20537=CARTESIAN_POINT('Ctrl Pts',(14.2111495086891,-0.349599823817769,
4.34595547117883));
#20538=CARTESIAN_POINT('Ctrl Pts',(14.258865344752,-0.480069828122688,3.8930505494253));
#20539=CARTESIAN_POINT('Ctrl Pts',(14.3065811808148,-0.169684322438749,
3.53835895376334));
#20540=CARTESIAN_POINT('Ctrl Pts',(14.3542970168777,0.296524907469595,3.60759943412104));
#20541=CARTESIAN_POINT('Ctrl Pts',(14.4020128529405,0.49043075222644,4.0371873919842));
#20542=CARTESIAN_POINT('Ctrl Pts',(14.4497286890033,0.233966490966644,4.43262559558668));
#20543=CARTESIAN_POINT('Ctrl Pts',(14.4974445250662,-0.237352798985028,
4.43077705796148));
#20544=CARTESIAN_POINT('Ctrl Pts',(14.545160361129,-0.490707361486496,4.03333931965322));
#20545=CARTESIAN_POINT('Ctrl Pts',(14.5928761971918,-0.293437803431633,
3.60528557111603));
#20546=CARTESIAN_POINT('Ctrl Pts',(14.6405920332547,0.173300204635467,3.53970415608515));
#20547=CARTESIAN_POINT('Ctrl Pts',(14.6883078693175,0.480893968219416,3.89681949708321));
#20548=CARTESIAN_POINT('Ctrl Pts',(14.7360237053804,0.346875401282657,4.34868708154587));
#20549=CARTESIAN_POINT('Ctrl Pts',(14.7837395414432,-0.10568418401607,4.48034995378457));
#20550=CARTESIAN_POINT('Ctrl Pts',(14.831455377506,-0.461192356972643,4.17090007232882));
#20551=CARTESIAN_POINT('Ctrl Pts',(14.8791712135689,-0.393180492164677,
3.7045100248179));
#20552=CARTESIAN_POINT('Ctrl Pts',(14.9268870496317,0.0358950684576197,
3.50947296821438));
#20553=CARTESIAN_POINT('Ctrl Pts',(14.9746028856945,0.432007635398663,3.76489443262817));
#20554=CARTESIAN_POINT('Ctrl Pts',(15.0223187217574,0.431400943461215,4.23621695712364));
#20555=CARTESIAN_POINT('Ctrl Pts',(15.0700345578202,0.0346321271865876,
4.4906178152274));
#20556=CARTESIAN_POINT('Ctrl Pts',(15.1177503938831,-0.393939904367254,
4.2944767844824));
#20557=CARTESIAN_POINT('Ctrl Pts',(15.1654662299459,-0.46075086019608,3.82791319143947));
#20558=CARTESIAN_POINT('Ctrl Pts',(15.2131820660087,-0.104447211543591,
3.51937956259357));
#20559=CARTESIAN_POINT('Ctrl Pts',(15.2608979020716,0.347771918596306,3.652207076714));
#20560=CARTESIAN_POINT('Ctrl Pts',(15.3086137381344,0.480626744730421,4.10441818376995));
#20561=CARTESIAN_POINT('Ctrl Pts',(15.3563295741973,0.172114635785536,4.46074046598969));
#20562=CARTESIAN_POINT('Ctrl Pts',(15.4040454102601,-0.294452991525291,
4.39395768888776));
#20563=CARTESIAN_POINT('Ctrl Pts',(15.4517612463229,-0.490619905976795,
3.96539750426199));
#20564=CARTESIAN_POINT('Ctrl Pts',(15.4994770823858,-0.236243011612202,
3.56861332390027));
#20565=CARTESIAN_POINT('Ctrl Pts',(15.5471929184486,0.235079475381852,3.56797816593814));
#20566=CARTESIAN_POINT('Ctrl Pts',(15.5949087545115,0.490524862970081,3.9640753057054));
#20567=CARTESIAN_POINT('Ctrl Pts',(15.6426245905743,0.295513721197704,4.39316264501585));
#20568=CARTESIAN_POINT('Ctrl Pts',(15.6903404266371,-0.170872217813597,
4.46120267782338));
#20569=CARTESIAN_POINT('Ctrl Pts',(15.7380562626999,-0.480343569999647,
4.1057131950703));
#20570=CARTESIAN_POINT('Ctrl Pts',(15.7857720987628,-0.348708030819167,
3.6531456586776));
#20571=CARTESIAN_POINT('Ctrl Pts',(15.8334879348256,0.103151458625294,3.5190998009613));
#20572=CARTESIAN_POINT('Ctrl Pts',(15.8812037708885,0.460285376424935,3.82667199562295));
#20573=CARTESIAN_POINT('Ctrl Pts',(15.9289196069513,0.39473215065269,4.29341396369818));
#20574=CARTESIAN_POINT('Ctrl Pts',(15.9766354430142,-0.033309682798763,
4.49070937415524));
#20575=CARTESIAN_POINT('Ctrl Pts',(16.024351279077,-0.430762722000766,4.23737881579128));
#20576=CARTESIAN_POINT('Ctrl Pts',(16.0720671151398,-0.432639725453012,
3.76605963834362));
#20577=CARTESIAN_POINT('Ctrl Pts',(16.1197829512026,-0.0372170120039125,
3.50957149464017));
#20578=CARTESIAN_POINT('Ctrl Pts',(16.1674987872655,0.392382656225717,3.70345139362117));
#20579=CARTESIAN_POINT('Ctrl Pts',(16.2152146233283,0.461651293660056,4.16965644082667));
#20580=CARTESIAN_POINT('Ctrl Pts',(16.2629304593912,0.106978444708158,4.48006336792116));
#20581=CARTESIAN_POINT('Ctrl Pts',(16.310646295454,-0.345934356094203,4.34962071752925));
#20582=CARTESIAN_POINT('Ctrl Pts',(16.3583621315169,-0.481170314810987,
3.89811598262401));
#20583=CARTESIAN_POINT('Ctrl Pts',(16.4060779675797,-0.174540169679895,
3.54017290856226));
#20584=CARTESIAN_POINT('Ctrl Pts',(16.4537938036425,0.292372898913969,3.60449612791703));
#20585=CARTESIAN_POINT('Ctrl Pts',(16.5015096397054,0.490795435699827,4.0320166386149));
#20586=CARTESIAN_POINT('Ctrl Pts',(16.5492254757682,0.238512972024049,4.4301357774334));
#20587=CARTESIAN_POINT('Ctrl Pts',(16.596941311831,-0.23279962385521,4.43325461334514));
#20588=CARTESIAN_POINT('Ctrl Pts',(16.6446571478939,-0.490328743065594,
4.03850907134293));
#20589=CARTESIAN_POINT('Ctrl Pts',(16.6923729839567,-0.297581432841348,
3.60840005658827));
#20590=CARTESIAN_POINT('Ctrl Pts',(16.7400888200196,0.168439486040012,3.53790329540825));
#20591=CARTESIAN_POINT('Ctrl Pts',(16.7878046560824,0.479779833116189,3.89175704832657));
#20592=CARTESIAN_POINT('Ctrl Pts',(16.8355204921452,0.350530977080134,4.3450119692985));
#20593=CARTESIAN_POINT('Ctrl Pts',(16.8832363282081,-0.100615868820984,
4.4814370901721));
#20594=CARTESIAN_POINT('Ctrl Pts',(16.9309521642709,-0.459365614209645,
4.17575112327883));
#20595=CARTESIAN_POINT('Ctrl Pts',(16.9786680003337,-0.396272847821079,
3.70867019559999));
#20596=CARTESIAN_POINT('Ctrl Pts',(17.0263838363966,0.0307233721630972,
3.5091219099869));
#20597=CARTESIAN_POINT('Ctrl Pts',(17.0740996724594,0.429505846750062,3.76035452756312));
#20598=CARTESIAN_POINT('Ctrl Pts',(17.1218155085223,0.433866493469502,4.23165726989771));
#20599=CARTESIAN_POINT('Ctrl Pts',(17.1695313445851,0.039800863341802,4.49022557677993));
#20600=CARTESIAN_POINT('Ctrl Pts',(17.217247180648,-0.390814512007675,4.29861219341511));
#20601=CARTESIAN_POINT('Ctrl Pts',(17.2649630167107,-0.462538907526291,
3.83277863809798));
#20602=CARTESIAN_POINT('Ctrl Pts',(17.3126788527736,-0.109506707187599,
3.52050703244687));
#20603=CARTESIAN_POINT('Ctrl Pts',(17.3603946888365,0.344087187338735,3.64856119684745));
#20604=CARTESIAN_POINT('Ctrl Pts',(17.4081105248993,0.481700523269991,4.09934702176407));
#20605=CARTESIAN_POINT('Ctrl Pts',(17.4558263609621,0.176960856767158,4.45890094794434));
#20606=CARTESIAN_POINT('Ctrl Pts',(17.503542197025,-0.290284687397741,4.39703907252861));
#20607=CARTESIAN_POINT('Ctrl Pts',(17.5512580330878,-0.490957336521241,
3.97057010757845));
#20608=CARTESIAN_POINT('Ctrl Pts',(17.5989738691507,-0.240776309167652,
3.57112706567612));
#20609=CARTESIAN_POINT('Ctrl Pts',(17.6466897052135,0.230513307714322,3.56552463842171));
#20610=CARTESIAN_POINT('Ctrl Pts',(17.6944055412763,0.490119007219086,3.95890762096741));
#20611=CARTESIAN_POINT('Ctrl Pts',(17.7421213773392,0.299640880944266,4.39002636746625));
#20612=CARTESIAN_POINT('Ctrl Pts',(17.789837213402,-0.166002076869247,4.46297789939377));
#20613=CARTESIAN_POINT('Ctrl Pts',(17.8375530494648,-0.479202773223469,
4.11076970247734));
#20614=CARTESIAN_POINT('Ctrl Pts',(17.8852688855277,-0.352344189444135,
3.65683998336499));
#20615=CARTESIAN_POINT('Ctrl Pts',(17.9329847215905,0.0980774850139738,
3.51803938772416));
#20616=CARTESIAN_POINT('Ctrl Pts',(17.9807005576534,0.458433095867658,3.82183063825345));
#20617=CARTESIAN_POINT('Ctrl Pts',(18.0284163937162,0.397802540886209,4.28923755516265));
#20618=CARTESIAN_POINT('Ctrl Pts',(18.076132229779,-0.0281362083699241,
4.49103317467411));
#20619=CARTESIAN_POINT('Ctrl Pts',(18.1238480658419,-0.428237044548737,
4.24190547436581));
#20620=CARTESIAN_POINT('Ctrl Pts',(18.1715639019047,-0.435081213444543,
3.7706322547532));
#20621=CARTESIAN_POINT('Ctrl Pts',(18.2192797379675,-0.0423836094492617,
3.50999096487715));
#20622=CARTESIAN_POINT('Ctrl Pts',(18.2669955740304,0.389235515258945,3.69933251171255));
#20623=CARTESIAN_POINT('Ctrl Pts',(18.3147114100932,0.463413677146622,4.16478163940629));
#20624=CARTESIAN_POINT('Ctrl Pts',(18.3624272461561,0.112031928774586,4.4789092521418));
#20625=CARTESIAN_POINT('Ctrl Pts',(18.4101430822189,-0.342230463623947,
4.35324712966946));
#20626=CARTESIAN_POINT('Ctrl Pts',(18.4578589182817,-0.482217355384067,
3.90319273261591));
#20627=CARTESIAN_POINT('Ctrl Pts',(18.5055747543446,-0.179376629827252,
3.54203793877243));
#20628=CARTESIAN_POINT('Ctrl Pts',(18.5532905904074,0.288188414964166,3.60143675240633));
#20629=CARTESIAN_POINT('Ctrl Pts',(18.6010064264702,0.491105603945206,4.02684232898929));
#20630=CARTESIAN_POINT('Ctrl Pts',(18.6487222625331,0.243032960192409,4.42759818183915));
#20631=CARTESIAN_POINT('Ctrl Pts',(18.6964380985959,-0.228220590447982,
4.43568404486223));
#20632=CARTESIAN_POINT('Ctrl Pts',(18.7441539346588,-0.489895661254576,
4.0436745456279));
#20633=CARTESIAN_POINT('Ctrl Pts',(18.7918697707216,-0.301692008317894,
3.6115580391236));
#20634=CARTESIAN_POINT('Ctrl Pts',(18.8395856067845,0.163560057986223,3.53615376224111));
#20635=CARTESIAN_POINT('Ctrl Pts',(18.8873014428472,0.478612406344963,3.88670662268212));
#20636=CARTESIAN_POINT('Ctrl Pts',(18.9350172789101,0.35414761756175,4.34129853476112));
#20637=CARTESIAN_POINT('Ctrl Pts',(18.982733114973,-0.0955363776958117,
4.48247075080787));
#20638=CARTESIAN_POINT('Ctrl Pts',(19.0304489510358,-0.457487847288108,
4.18058265263639));
#20639=CARTESIAN_POINT('Ctrl Pts',(19.0781647870987,-0.399321187381313,
3.71286272589862));
#20640=CARTESIAN_POINT('Ctrl Pts',(19.1258806231614,0.0255482632835279,
3.50882537619781));
#20641=CARTESIAN_POINT('Ctrl Pts',(19.1735964592243,0.426956350589889,3.75584124112414));
#20642=CARTESIAN_POINT('Ctrl Pts',(19.2213122952871,0.436283851722622,4.22707185138688));
#20643=CARTESIAN_POINT('Ctrl Pts',(19.26902813135,0.0449651784623906,4.48977888620274));
#20644=CARTESIAN_POINT('Ctrl Pts',(19.3167439674128,-0.387645709555542,
4.3027144342981));
#20645=CARTESIAN_POINT('Ctrl Pts',(19.3644598034757,-0.464275578741542,
3.8376626582024));
#20646=CARTESIAN_POINT('Ctrl Pts',(19.4121756395385,-0.114554038379521,
3.52168776344319));
#20647=CARTESIAN_POINT('Ctrl Pts',(19.4598914756013,0.340364234683876,3.64495435060606));
#20648=CARTESIAN_POINT('Ctrl Pts',(19.5076073116642,0.482720800247919,4.09426482953845));
#20649=CARTESIAN_POINT('Ctrl Pts',(19.555323147727,0.181787415268628,4.45701044834135));
#20650=CARTESIAN_POINT('Ctrl Pts',(19.6030389837899,-0.28608412753634,4.40007637198121));
#20651=CARTESIAN_POINT('Ctrl Pts',(19.6507548198527,-0.491240257057309,
3.97574594767572));
#20652=CARTESIAN_POINT('Ctrl Pts',(19.6984706559155,-0.245282818621706,
3.57368850533185));
#20653=CARTESIAN_POINT('Ctrl Pts',(19.7461864919783,0.225921452997342,3.56311925573479));
#20654=CARTESIAN_POINT('Ctrl Pts',(19.7939023280412,0.489658867576397,3.95374471702426));
#20655=CARTESIAN_POINT('Ctrl Pts',(19.841618164104,0.303734463062876,4.38684635894002));
#20656=CARTESIAN_POINT('Ctrl Pts',(19.8893340001669,-0.161112940293692,
4.46470246728215));
#20657=CARTESIAN_POINT('Ctrl Pts',(19.9370498362297,-0.47800980043334,4.11581244897344));
#20658=CARTESIAN_POINT('Ctrl Pts',(19.9847656722926,-0.355939225796451,
3.66057517601247));
#20659=CARTESIAN_POINT('Ctrl Pts',(20.0324815083554,0.0929888682922082,
3.51702731322357));
#20660=CARTESIAN_POINT('Ctrl Pts',(20.0801973444182,0.456536973876988,3.81701888067549));
#20661=CARTESIAN_POINT('Ctrl Pts',(20.1279131804811,0.400815378068436,4.28501049648274));
#20662=CARTESIAN_POINT('Ctrl Pts',(20.1756290165439,-0.022934367574535,
4.49133741301101));
#20663=CARTESIAN_POINT('Ctrl Pts',(20.2233448526067,-0.425711472830213,
4.24633918020534));
#20664=CARTESIAN_POINT('Ctrl Pts',(20.2710606886696,-0.437384262562023,
3.77535541015343));
#20665=CARTESIAN_POINT('Ctrl Pts',(20.3187765247324,-0.0477164433392854,
3.51022640082505));
#20666=CARTESIAN_POINT('Ctrl Pts',(20.3664923607953,0.386374384143037,3.69571627142296));
#20667=CARTESIAN_POINT('Ctrl Pts',(20.4062555575143,0.45143962727185,4.08165775845481));
#20668=CARTESIAN_POINT('Ctrl Pts',(20.4380661148895,0.291471375703242,4.31996082336987));
#20669=CARTESIAN_POINT('Ctrl Pts',(20.461924032921,0.103697252552815,4.42124466395835));
#20670=CARTESIAN_POINT('Ctrl Pts',(20.4857819509523,-0.111451542568667,
4.41901444157942));
#20671=CARTESIAN_POINT('Ctrl Pts',(20.5096398689838,-0.298255971346869,
4.31460392554555));
#20672=CARTESIAN_POINT('Ctrl Pts',(20.5334977870152,-0.412709509332759,
4.13311446574462));
#20673=CARTESIAN_POINT('Ctrl Pts',(20.5573557050466,-0.425936384696969,
3.91915434697803));
#20674=CARTESIAN_POINT('Ctrl Pts',(20.581213623078,-0.335173342752607,3.72492109335083));
#20675=CARTESIAN_POINT('Ctrl Pts',(20.6050715411095,-0.162364888615448,
3.59797442377207));
#20676=CARTESIAN_POINT('Ctrl Pts',(20.6289294591408,0.0501004451364318,
3.56932214892951));
#20677=CARTESIAN_POINT('Ctrl Pts',(20.6527873771723,0.250339089241223,3.64598859455508));
#20678=CARTESIAN_POINT('Ctrl Pts',(20.6766452952037,0.389350172549011,3.80921715950176));
#20679=CARTESIAN_POINT('Ctrl Pts',(20.7005032132352,0.433161330121289,4.01909908002448));
#20680=CARTESIAN_POINT('Ctrl Pts',(20.7243611312665,0.371049143609512,4.22430982617278));
#20681=CARTESIAN_POINT('Ctrl Pts',(20.748219049298,0.218207240773441,4.37467120177868));
#20682=CARTESIAN_POINT('Ctrl Pts',(20.7720769673293,0.01200671405148,4.43341500212799));
#20683=CARTESIAN_POINT('Ctrl Pts',(20.7959348853608,-0.197129246586683,
4.38617716647524));
#20684=CARTESIAN_POINT('Ctrl Pts',(20.8197928033922,-0.358062019934396,
4.24450842127602));
#20685=CARTESIAN_POINT('Ctrl Pts',(20.8436507214237,-0.431438726014498,
4.04305074550709));
#20686=CARTESIAN_POINT('Ctrl Pts',(20.867508639455,-0.399316990859146,3.83106596928302));
#20687=CARTESIAN_POINT('Ctrl Pts',(20.8913665574865,-0.269551332195825,
3.66039017609669));
#20688=CARTESIAN_POINT('Ctrl Pts',(20.9152244755179,-0.0738730526583281,
3.57275822989076));
#20689=CARTESIAN_POINT('Ctrl Pts',(20.9390823935493,0.139869212314499,3.58959853735383));
#20690=CARTESIAN_POINT('Ctrl Pts',(20.9629403115807,0.319409638666883,3.70679317993256));
#20691=CARTESIAN_POINT('Ctrl Pts',(20.9867982296122,0.420845711130686,3.8956848776653));
#20692=CARTESIAN_POINT('Ctrl Pts',(21.0106561476436,0.419373541863394,4.11008446384341));
#20693=CARTESIAN_POINT('Ctrl Pts',(21.034514065675,0.315353119032788,4.29756540021079));
#20694=CARTESIAN_POINT('Ctrl Pts',(21.0583719837064,0.134220268060588,4.41228349058099));
#20695=CARTESIAN_POINT('Ctrl Pts',(21.0822299017379,-0.079733094278782,
4.42618703719455));
#20696=CARTESIAN_POINT('Ctrl Pts',(21.1060878197692,-0.274189543318984,
4.33587624407661));
#20697=CARTESIAN_POINT('Ctrl Pts',(21.1299457378007,-0.401599180171465,
4.16343456021562));
#20698=CARTESIAN_POINT('Ctrl Pts',(21.1538036558321,-0.430806878168669,
3.95102867450389));
#20699=CARTESIAN_POINT('Ctrl Pts',(21.1776615738635,-0.354670559489406,
3.75059761183336));
#20700=CARTESIAN_POINT('Ctrl Pts',(21.2015194918949,-0.191807627993766,
3.61115222665144));
#20701=CARTESIAN_POINT('Ctrl Pts',(21.2253774099264,0.0179574932869785,
3.56679071405539));
#20702=CARTESIAN_POINT('Ctrl Pts',(21.2492353279577,0.223331518303719,3.62836067225603));
#20703=CARTESIAN_POINT('Ctrl Pts',(21.2730932459892,0.374094903668402,3.78080656934254));
#20704=CARTESIAN_POINT('Ctrl Pts',(21.2969511640206,0.433381894944723,3.98685123093373));
#20705=CARTESIAN_POINT('Ctrl Pts',(21.320809082052,0.386695207821707,4.19611112472705));
#20706=CARTESIAN_POINT('Ctrl Pts',(21.3446670000834,0.245451009020076,4.35741650656472));
#20707=CARTESIAN_POINT('Ctrl Pts',(21.3685249181149,0.0441873525619181,
4.43132381671722));
#20708=CARTESIAN_POINT('Ctrl Pts',(21.3923828361462,-0.167881315237013,
4.39976070465745));
#20709=CARTESIAN_POINT('Ctrl Pts',(21.4162407541777,-0.338898428465248,
4.27044521104599));
#20710=CARTESIAN_POINT('Ctrl Pts',(21.4400986722091,-0.427045644525908,
4.07499849655415));
#20711=CARTESIAN_POINT('Ctrl Pts',(21.4639565902406,-0.410768568010174,
3.86121260673678));
#20712=CARTESIAN_POINT('Ctrl Pts',(21.4878145082719,-0.294047387504818,
3.68136401506497));
#20713=CARTESIAN_POINT('Ctrl Pts',(21.5116724263034,-0.105423611064507,
3.57943060117972));
#20714=CARTESIAN_POINT('Ctrl Pts',(21.5355303443348,0.108979109962582,3.58033786138646));
#20715=CARTESIAN_POINT('Ctrl Pts',(21.5593882623662,0.296733470072461,3.68386394585134));
#20716=CARTESIAN_POINT('Ctrl Pts',(21.5832461803976,0.411928413892185,3.86469390692879));
#20717=CARTESIAN_POINT('Ctrl Pts',(21.6071040984291,0.426395639810567,4.07860989342611));
#20718=CARTESIAN_POINT('Ctrl Pts',(21.6309620164605,0.33659751701124,4.27330361969026));
#20719=CARTESIAN_POINT('Ctrl Pts',(21.6548199344919,0.164492132570386,4.401167166299));
#20720=CARTESIAN_POINT('Ctrl Pts',(21.6786778525233,-0.0478360589596606,
4.43093441317345));
#20721=CARTESIAN_POINT('Ctrl Pts',(21.7025357705547,-0.248467031045983,
4.35532645760922));
#20722=CARTESIAN_POINT('Ctrl Pts',(21.7263936885861,-0.388341045935521,
4.1928315042612));
#20723=CARTESIAN_POINT('Ctrl Pts',(21.7502516066176,-0.433255096896122,
3.98318399549658));
#20724=CARTESIAN_POINT('Ctrl Pts',(21.774109524649,-0.372226475033738,3.77764845789182));
#20725=CARTESIAN_POINT('Ctrl Pts',(21.7979674426804,-0.220178340780001,
3.62648392906691));
#20726=CARTESIAN_POINT('Ctrl Pts',(21.8218253607118,-0.0142906046679706,
3.56665425395863));
#20727=CARTESIAN_POINT('Ctrl Pts',(21.8456832787432,0.195091573553633,3.61278941785858));
#20728=CARTESIAN_POINT('Ctrl Pts',(21.8695411967747,0.356768547853618,3.75360811649661));
#20729=CARTESIAN_POINT('Ctrl Pts',(21.8933991148061,0.431205894023261,3.95467634223136));
#20730=CARTESIAN_POINT('Ctrl Pts',(21.9172570328375,0.400201653291494,4.16682743688221));
#20731=CARTESIAN_POINT('Ctrl Pts',(21.941114950869,0.271337207055788,4.33818467892719));
#20732=CARTESIAN_POINT('Ctrl Pts',(21.9649728689003,0.0761234226178432,
4.4268465550088));
#20733=CARTESIAN_POINT('Ctrl Pts',(21.9888307869318,-0.137704612210607,
4.41113282132402));
#20734=CARTESIAN_POINT('Ctrl Pts',(22.0126887049632,-0.317860118355158,
4.29488591379237));
#20735=CARTESIAN_POINT('Ctrl Pts',(22.0365466229946,-0.420290167226249,
4.10653136780738));
#20736=CARTESIAN_POINT('Ctrl Pts',(22.060404541026,-0.419947821735935,3.89212700053744));
#20737=CARTESIAN_POINT('Ctrl Pts',(22.0842624590574,-0.316916794682727,
3.70410052003731));
#20738=CARTESIAN_POINT('Ctrl Pts',(22.1081203770888,-0.136390978688423,
3.58842952252864));
#20739=CARTESIAN_POINT('Ctrl Pts',(22.1319782951203,0.0774861468089536,
3.57339871771534));
#20740=CARTESIAN_POINT('Ctrl Pts',(22.1558362131517,0.27241579873489,3.66268354680831));
#20741=CARTESIAN_POINT('Ctrl Pts',(22.1796941311831,0.400732367405962,3.83445143701846));
#20742=CARTESIAN_POINT('Ctrl Pts',(22.2035520492145,0.431058956528623,4.04670046033727));
#20743=CARTESIAN_POINT('Ctrl Pts',(22.227409967246,0.355979888945518,4.24752994899471));
#20744=CARTESIAN_POINT('Ctrl Pts',(22.2512678852773,0.193854041863619,4.38783162256878));
#20745=CARTESIAN_POINT('Ctrl Pts',(22.2751258033088,-0.0156743990186396,
4.43329790005389));
#20746=CARTESIAN_POINT('Ctrl Pts',(22.2989837213402,-0.221370022215225,
4.37281103827166));
#20747=CARTESIAN_POINT('Ctrl Pts',(22.3228416393716,-0.372934645290675,
4.22116172228637));
#20748=CARTESIAN_POINT('Ctrl Pts',(22.346699557403,-0.43330658847365,4.01543234121164));
#20749=CARTESIAN_POINT('Ctrl Pts',(22.3705574754345,-0.387723268841402,
3.80592933171158));
#20750=CARTESIAN_POINT('Ctrl Pts',(22.3944153934659,-0.247331046528593,
3.64388188817752));
#20751=CARTESIAN_POINT('Ctrl Pts',(22.4182733114973,-0.0464596501027702,
3.56891502119853));
#20752=CARTESIAN_POINT('Ctrl Pts',(22.4421312295287,0.165772403721094,3.59936017830047));
#20753=CARTESIAN_POINT('Ctrl Pts',(22.4659891475602,0.337468575289321,3.7277726770023));
#20754=CARTESIAN_POINT('Ctrl Pts',(22.4898470655915,0.426644514167594,3.92275218663495));
#20755=CARTESIAN_POINT('Ctrl Pts',(22.513704983623,0.411494197867752,4.13662086224655));
#20756=CARTESIAN_POINT('Ctrl Pts',(22.5375629016544,0.295722435535401,4.31708206952049));
#20757=CARTESIAN_POINT('Ctrl Pts',(22.5614208196858,0.107638304484935,4.42000797176855));
#20758=CARTESIAN_POINT('Ctrl Pts',(22.5852787377172,-0.106765988085903,
4.42023067651324));
#20759=CARTESIAN_POINT('Ctrl Pts',(22.6091366557487,-0.295063722636797,
4.31769517074077));
#20760=CARTESIAN_POINT('Ctrl Pts',(22.6329945737801,-0.411209141905604,
4.13747522778479));
#20761=CARTESIAN_POINT('Ctrl Pts',(22.6568524918115,-0.426804986482714,
3.92363755172126));
#20762=CARTESIAN_POINT('Ctrl Pts',(22.6807104098429,-0.33803111495158,3.72847502015617));
#20763=CARTESIAN_POINT('Ctrl Pts',(22.7045683278743,-0.16660749730952,3.59970312177549));
#20764=CARTESIAN_POINT('Ctrl Pts',(22.7284262459057,0.0455714674079685,
3.56882345794434));
#20765=CARTESIAN_POINT('Ctrl Pts',(22.7522841639372,0.246577802732478,3.64336153500176));
#20766=CARTESIAN_POINT('Ctrl Pts',(22.7761420819686,0.387346815298129,3.80514019809748));
#20767=CARTESIAN_POINT('Ctrl Pts',(22.7920473606562,0.417963038852713,3.94471011778788));
#20768=CARTESIAN_POINT('Ctrl Pts',(22.8,0.415641328671541,4.01393920819689));
#20769=CARTESIAN_POINT('Ctrl Pts',(3.96816317011929,0.203757107801821,4.42939176513376));
#20770=CARTESIAN_POINT('Ctrl Pts',(3.9761158094631,0.132237748973037,4.46332948562603));
#20771=CARTESIAN_POINT('Ctrl Pts',(3.99202108815071,-0.0280119004087947,
4.49474661085258));
#20772=CARTESIAN_POINT('Ctrl Pts',(4.01587900618213,-0.261670681609628,
4.42079217330492));
#20773=CARTESIAN_POINT('Ctrl Pts',(4.03973692421355,-0.431283260509235,
4.24398813071681));
#20774=CARTESIAN_POINT('Ctrl Pts',(4.06359484224497,-0.495466080430727,
4.00749935521381));
#20775=CARTESIAN_POINT('Ctrl Pts',(4.08745276027639,-0.438477829352452,
3.76918881818141));
#20776=CARTESIAN_POINT('Ctrl Pts',(4.11131067830781,-0.274278321106756,
3.5873115455631));
#20777=CARTESIAN_POINT('Ctrl Pts',(4.13516859633923,-0.0430057845205295,
3.50635120590702));
#20778=CARTESIAN_POINT('Ctrl Pts',(4.15902651437064,0.198780450874126,3.54609966156282));
#20779=CARTESIAN_POINT('Ctrl Pts',(4.18288443240206,0.391960715466274,3.69684005745713));
#20780=CARTESIAN_POINT('Ctrl Pts',(4.20674235043348,0.489295238859844,3.92171081754005));
#20781=CARTESIAN_POINT('Ctrl Pts',(4.2306002684649,0.466984102771714,4.16572567991789));
#20782=CARTESIAN_POINT('Ctrl Pts',(4.25445818649632,0.330482445391075,4.36921595913043));
#20783=CARTESIAN_POINT('Ctrl Pts',(4.27831610452774,0.113168927396708,4.48242295331799));
#20784=CARTESIAN_POINT('Ctrl Pts',(4.30217402255916,-0.131817528672551,
4.47766435517297));
#20785=CARTESIAN_POINT('Ctrl Pts',(4.32603194059057,-0.344570980451485,
4.35610383169054));
#20786=CARTESIAN_POINT('Ctrl Pts',(4.349889858622,-0.473067456356951,4.14746621026076));
#20787=CARTESIAN_POINT('Ctrl Pts',(4.37374777665341,-0.485886045261059,
3.9027690893624));
#20788=CARTESIAN_POINT('Ctrl Pts',(4.39760569468484,-0.379892264971952,
3.68184757153936));
#20789=CARTESIAN_POINT('Ctrl Pts',(4.42146361271625,-0.181004475645389,
3.53872299041084));
#20790=CARTESIAN_POINT('Ctrl Pts',(4.44532153074767,0.0621438372772935,
3.50839320219298));
#20791=CARTESIAN_POINT('Ctrl Pts',(4.46917944877909,0.290096289836991,3.5982746675986));
#20792=CARTESIAN_POINT('Ctrl Pts',(4.49303736681051,0.447112297141319,3.78638891931142));
#20793=CARTESIAN_POINT('Ctrl Pts',(4.51689528484194,0.494797168872773,4.02673689903048));
#20794=CARTESIAN_POINT('Ctrl Pts',(4.54075320287334,0.421490654719143,4.26054697856981));
#20795=CARTESIAN_POINT('Ctrl Pts',(4.56461112090478,0.245118194360182,4.43064622472778));
#20796=CARTESIAN_POINT('Ctrl Pts',(4.58846903893618,0.00880765856895839,
4.49544073835303));
#20797=CARTESIAN_POINT('Ctrl Pts',(4.61232695696761,-0.229656589644598,
4.43908649592634));
#20798=CARTESIAN_POINT('Ctrl Pts',(4.63618487499902,-0.411963545977342,
4.2753636447643));
#20799=CARTESIAN_POINT('Ctrl Pts',(4.66004279303045,-0.493534193653132,
4.04430688170513));
#20800=CARTESIAN_POINT('Ctrl Pts',(4.68390071106186,-0.454422287381232,
3.80241587917234));
#20801=CARTESIAN_POINT('Ctrl Pts',(4.70775862909328,-0.304191753628974,
3.60883957626609));
#20802=CARTESIAN_POINT('Ctrl Pts',(4.7316165471247,-0.0795780500979935,
3.51091265195837));
#20803=CARTESIAN_POINT('Ctrl Pts',(4.75547446515612,0.164494654344808,3.53258090671894));
#20804=CARTESIAN_POINT('Ctrl Pts',(4.77933238318754,0.368343935055725,3.66854586202706));
#20805=CARTESIAN_POINT('Ctrl Pts',(4.80319030121895,0.482123090158262,3.88556038269908));
#20806=CARTESIAN_POINT('Ctrl Pts',(4.82704821925038,0.478010016947761,4.13055850707372));
#20807=CARTESIAN_POINT('Ctrl Pts',(4.85090613728179,0.357010473862124,4.34363152012653));
#20808=CARTESIAN_POINT('Ctrl Pts',(4.87476405531322,0.14871214514713,4.47267726617372));
#20809=CARTESIAN_POINT('Ctrl Pts',(4.89862197334463,-0.0959503538938319,
4.48614054517122));
#20810=CARTESIAN_POINT('Ctrl Pts',(4.92247989137606,-0.317150377772593,
4.38072921867179));
#20811=CARTESIAN_POINT('Ctrl Pts',(4.94633780940747,-0.460798495283114,
4.1822192273514));
#20812=CARTESIAN_POINT('Ctrl Pts',(4.97019572743889,-0.49176882879792,3.93915167139151));
#20813=CARTESIAN_POINT('Ctrl Pts',(4.99405364547031,-0.40248828815769,3.71096318925158));
#20814=CARTESIAN_POINT('Ctrl Pts',(5.01791156350173,-0.214788397502062,
3.55345208054429));
#20815=CARTESIAN_POINT('Ctrl Pts',(5.04176948153314,0.0254331070612992,
3.50513410186502));
#20816=CARTESIAN_POINT('Ctrl Pts',(5.06562739956457,0.259435524164246,3.57782431515618));
#20817=CARTESIAN_POINT('Ctrl Pts',(5.08948531759598,0.429998888727244,3.75374798322641));
#20818=CARTESIAN_POINT('Ctrl Pts',(5.11334323562741,0.495415812061873,3.98988697716804));
#20819=CARTESIAN_POINT('Ctrl Pts',(5.13720115365882,0.439690074491602,4.2284988806653));
#20820=CARTESIAN_POINT('Ctrl Pts',(5.16105907169025,0.276448136790977,4.41123658365534));
#20821=CARTESIAN_POINT('Ctrl Pts',(5.18491698972166,0.0456070993489057,
4.49341574008204));
#20822=CARTESIAN_POINT('Ctrl Pts',(5.20877490775308,-0.196386116196418,
4.45494130768376));
#20823=CARTESIAN_POINT('Ctrl Pts',(5.2326328257845,-0.390357576881318,4.3052213332044));
#20824=CARTESIAN_POINT('Ctrl Pts',(5.25649074381592,-0.488875976891831,
4.08086642869437));
#20825=CARTESIAN_POINT('Ctrl Pts',(5.28034866184734,-0.467850883838054,
3.83673747961128));
#20826=CARTESIAN_POINT('Ctrl Pts',(5.30420657987876,-0.332423505683668,
3.632530663945));
#20827=CARTESIAN_POINT('Ctrl Pts',(5.32806449791017,-0.115709525355139,
3.5181801106079));
#20828=CARTESIAN_POINT('Ctrl Pts',(5.3519224159416,0.129298585786916,3.52164764473745));
#20829=CARTESIAN_POINT('Ctrl Pts',(5.37578033397301,0.342689670681295,3.64208535978523));
#20830=CARTESIAN_POINT('Ctrl Pts',(5.39963825200445,0.472283796414913,3.85004295376459));
#20831=CARTESIAN_POINT('Ctrl Pts',(5.42349617003584,0.48639166917272,4.09466913029638));
#20832=CARTESIAN_POINT('Ctrl Pts',(5.44735408806728,0.381563529774833,4.31614612573549));
#20833=CARTESIAN_POINT('Ctrl Pts',(5.47121200609869,0.183432713764955,4.46031678178449));
#20834=CARTESIAN_POINT('Ctrl Pts',(5.49506992413012,-0.059552397366927,
4.49192744591021));
#20835=CARTESIAN_POINT('Ctrl Pts',(5.51892784216153,-0.287975325168481,
4.40324844967551));
#20836=CARTESIAN_POINT('Ctrl Pts',(5.54278576019295,-0.445980441674811,
4.21596422322942));
#20837=CARTESIAN_POINT('Ctrl Pts',(5.56664367822437,-0.494931191930538,
3.97587086145358));
#20838=CARTESIAN_POINT('Ctrl Pts',(5.59050159625579,-0.422857784100094,
3.74167773132221));
#20839=CARTESIAN_POINT('Ctrl Pts',(5.61435951428721,-0.247384129650275,
3.57065143242979));
#20840=CARTESIAN_POINT('Ctrl Pts',(5.63821743231862,-0.0114183168777074,
3.50461255354752));
#20841=CARTESIAN_POINT('Ctrl Pts',(5.66207535035005,0.227339585372105,3.55970939936999));
#20842=CARTESIAN_POINT('Ctrl Pts',(5.68593326838146,0.410506766445453,3.72246929038963));
#20843=CARTESIAN_POINT('Ctrl Pts',(5.70979118641288,0.493293861043031,3.9530929995654));
#20844=CARTESIAN_POINT('Ctrl Pts',(5.73364910444431,0.455457169749513,4.19518674831082));
#20845=CARTESIAN_POINT('Ctrl Pts',(5.75750702247572,0.306248793691327,4.38955201985635));
#20846=CARTESIAN_POINT('Ctrl Pts',(5.78136494050715,0.0821542461994931,
4.48866121222712));
#20847=CARTESIAN_POINT('Ctrl Pts',(5.80522285853855,-0.162029253596618,
4.46827942571263));
#20848=CARTESIAN_POINT('Ctrl Pts',(5.82908077656998,-0.366592184898752,
4.33339056701663));
#20849=CARTESIAN_POINT('Ctrl Pts',(5.85293869460139,-0.481513345756758,
4.11697862749145));
#20850=CARTESIAN_POINT('Ctrl Pts',(5.87679661263282,-0.478691368855474,
3.87196223809426));
#20851=CARTESIAN_POINT('Ctrl Pts',(5.90065453066423,-0.358816329143926,
3.65825454842257));
#20852=CARTESIAN_POINT('Ctrl Pts',(5.92451244869565,-0.151200892471453,
3.52811296978032));
#20853=CARTESIAN_POINT('Ctrl Pts',(5.94837036672708,0.093387223403125,3.5133605500302));
#20854=CARTESIAN_POINT('Ctrl Pts',(5.97222828475848,0.315139728168714,3.61760487120619));
#20855=CARTESIAN_POINT('Ctrl Pts',(5.99608620278992,0.459831779670103,3.81535495398299));
#20856=CARTESIAN_POINT('Ctrl Pts',(6.01994412082132,0.492082823488737,4.05825627791571));
#20857=CARTESIAN_POINT('Ctrl Pts',(6.04380203885276,0.404005480250355,4.28691141512903));
#20858=CARTESIAN_POINT('Ctrl Pts',(6.06765995688416,0.21713917558903,4.44541067075535));
#20859=CARTESIAN_POINT('Ctrl Pts',(6.09151787491559,-0.0228261843714051,
4.49499153360272));
#20860=CARTESIAN_POINT('Ctrl Pts',(6.11537579294701,-0.257204988275768,
4.42353981062321));
#20861=CARTESIAN_POINT('Ctrl Pts',(6.13923371097843,-0.428699479426561,
4.24850911946619));
#20862=CARTESIAN_POINT('Ctrl Pts',(6.16309162900984,-0.49534768549136,4.01273373861842));
#20863=CARTESIAN_POINT('Ctrl Pts',(6.18694954704127,-0.440903093044182,
3.77380201544612));
#20864=CARTESIAN_POINT('Ctrl Pts',(6.21080746507268,-0.278582990390117,
3.59026229064107));
#20865=CARTESIAN_POINT('Ctrl Pts',(6.23466538310411,-0.048260127889517,
3.50676273730504));
#20866=CARTESIAN_POINT('Ctrl Pts',(6.25852330113552,0.194087080856728,3.5441598063702));
#20867=CARTESIAN_POINT('Ctrl Pts',(6.28238121916694,0.388553448942855,3.69248145192407));
#20868=CARTESIAN_POINT('Ctrl Pts',(6.30623913719837,0.488798280742691,3.9170164641697));
#20869=CARTESIAN_POINT('Ctrl Pts',(6.33009705522977,0.468067515948433,4.15995908608738));
#20870=CARTESIAN_POINT('Ctrl Pts',(6.36190761260502,0.291040001689194,4.43610431491443));
#20871=CARTESIAN_POINT('Ctrl Pts',(6.40167080932402,-0.143168317426403,
4.54352222151223));
#20872=CARTESIAN_POINT('Ctrl Pts',(6.44938664538688,-0.535165231989368,
4.17285582464912));
#20873=CARTESIAN_POINT('Ctrl Pts',(6.49710248144971,-0.434543251113388,
3.64369891234367));
#20874=CARTESIAN_POINT('Ctrl Pts',(6.54481831751255,0.0645215567551043,
3.4416075490323));
#20875=CARTESIAN_POINT('Ctrl Pts',(6.59253415357539,0.504653900644641,3.75236619672659));
#20876=CARTESIAN_POINT('Ctrl Pts',(6.64024998963822,0.481186238846835,4.29049388273239));
#20877=CARTESIAN_POINT('Ctrl Pts',(6.68796582570107,0.01592709648968,4.56187610740764));
#20878=CARTESIAN_POINT('Ctrl Pts',(6.7356816617639,-0.464005405879062,4.31726850783359));
#20879=CARTESIAN_POINT('Ctrl Pts',(6.78339749782674,-0.517809574500644,
3.78131383674221));
#20880=CARTESIAN_POINT('Ctrl Pts',(6.83111333388957,-0.0961144992151805,
3.44617913151078));
#20881=CARTESIAN_POINT('Ctrl Pts',(6.87882916995242,0.413851019972934,3.61962818876606));
#20882=CARTESIAN_POINT('Ctrl Pts',(6.92654500601525,0.543767061592725,4.14237771887731));
#20883=CARTESIAN_POINT('Ctrl Pts',(6.97426084207809,0.174335412693353,4.53438003016987));
#20884=CARTESIAN_POINT('Ctrl Pts',(7.02197667814094,-0.355192171006393,
4.43565270890428));
#20885=CARTESIAN_POINT('Ctrl Pts',(7.06969251420376,-0.558540766450571,
3.93685892261342));
#20886=CARTESIAN_POINT('Ctrl Pts',(7.11740835026661,-0.248973074301851,
3.49604849518665));
#20887=CARTESIAN_POINT('Ctrl Pts',(7.16512418632944,0.289230577826905,3.51802452284194));
#20888=CARTESIAN_POINT('Ctrl Pts',(7.21284002239229,0.561829257914175,3.98260602935256));
#20889=CARTESIAN_POINT('Ctrl Pts',(7.26055585845511,0.318491529052478,4.46316069626365));
#20890=CARTESIAN_POINT('Ctrl Pts',(7.30827169451797,-0.217321894570402,
4.51838776411367));
#20891=CARTESIAN_POINT('Ctrl Pts',(7.35598753058078,-0.553565266295818,
4.09757137442565));
#20892=CARTESIAN_POINT('Ctrl Pts',(7.40370336664365,-0.381461142739227,
3.58715368886071));
#20893=CARTESIAN_POINT('Ctrl Pts',(7.45141920270646,0.140944621146953,3.45585912402047));
#20894=CARTESIAN_POINT('Ctrl Pts',(7.49913503876933,0.533918768911932,3.82425749787944));
#20895=CARTESIAN_POINT('Ctrl Pts',(7.54685087483214,0.436587096747522,4.3540429157916));
#20896=CARTESIAN_POINT('Ctrl Pts',(7.594566710895,-0.0616692246238245,4.5587052763707));
#20897=CARTESIAN_POINT('Ctrl Pts',(7.64228254695782,-0.503293747851232,
4.25029998493175));
#20898=CARTESIAN_POINT('Ctrl Pts',(7.68999838302067,-0.482735878399531,
3.7120403659385));
#20899=CARTESIAN_POINT('Ctrl Pts',(7.7377142190835,-0.0188742238918736,
3.43821850974892));
#20900=CARTESIAN_POINT('Ctrl Pts',(7.78543005514633,0.462319920793015,3.6802892401675));
#20901=CARTESIAN_POINT('Ctrl Pts',(7.83314589120918,0.518958568528469,4.21595528072725));
#20902=CARTESIAN_POINT('Ctrl Pts',(7.88086172727202,0.099029577569048,4.55330626409362));
#20903=CARTESIAN_POINT('Ctrl Pts',(7.92857756333485,-0.411839798232008,
4.38254759143289));
#20904=CARTESIAN_POINT('Ctrl Pts',(7.9762933993977,-0.544510350349916,3.86048957930736));
#20905=CARTESIAN_POINT('Ctrl Pts',(8.02400923546053,-0.177148669371157,
3.466546133148));
#20906=CARTESIAN_POINT('Ctrl Pts',(8.07172507152338,0.352891360472903,3.56248158116143));
#20907=CARTESIAN_POINT('Ctrl Pts',(8.1194409075862,0.558865824063627,4.06019692528064));
#20908=CARTESIAN_POINT('Ctrl Pts',(8.16715674364906,0.251625202160443,4.50263250666582));
#20909=CARTESIAN_POINT('Ctrl Pts',(8.21487257971187,-0.286686714637947,
4.48349292318459));
#20910=CARTESIAN_POINT('Ctrl Pts',(8.26258841577472,-0.561729810142263,
4.02035434884804));
#20911=CARTESIAN_POINT('Ctrl Pts',(8.31030425183756,-0.32092777766878,3.53852406277244));
#20912=CARTESIAN_POINT('Ctrl Pts',(8.3580200879004,0.21458717114652,3.4804742305729));
#20913=CARTESIAN_POINT('Ctrl Pts',(8.40573592396324,0.553043418849938,3.89951290636976));
#20914=CARTESIAN_POINT('Ctrl Pts',(8.45345176002607,0.383631385356639,4.41083042643994));
#20915=CARTESIAN_POINT('Ctrl Pts',(8.50116759608892,-0.13807525223727,4.54487604447167));
#20916=CARTESIAN_POINT('Ctrl Pts',(8.54888343215175,-0.532985261140852,
4.17855360686946));
#20917=CARTESIAN_POINT('Ctrl Pts',(8.59659926821459,-0.43844670370641,3.64826264467864));
#20918=CARTESIAN_POINT('Ctrl Pts',(8.64431510427743,0.0587242081113278,
3.4409775080543));
#20919=CARTESIAN_POINT('Ctrl Pts',(8.69203094034026,0.501967776032349,3.74705132745037));
#20920=CARTESIAN_POINT('Ctrl Pts',(8.73974677640311,0.484246611455832,4.28541180496438));
#20921=CARTESIAN_POINT('Ctrl Pts',(8.78746261246592,0.021834332487559,4.56167423035448));
#20922=CARTESIAN_POINT('Ctrl Pts',(8.83517844852879,-0.460628749968427,
4.32214256754115));
#20923=CARTESIAN_POINT('Ctrl Pts',(8.88289428459161,-0.520089363644054,
3.78678242815423));
#20924=CARTESIAN_POINT('Ctrl Pts',(8.93061012065447,-0.101943912081849,
3.44722326576734));
#20925=CARTESIAN_POINT('Ctrl Pts',(8.97832595671729,0.409818202553832,3.61528748398963));
#20926=CARTESIAN_POINT('Ctrl Pts',(9.02604179278014,0.545237955920739,4.1366391252272));
#20927=CARTESIAN_POINT('Ctrl Pts',(9.07375762884296,0.179957304801303,4.53251295530543));
#20928=CARTESIAN_POINT('Ctrl Pts',(9.12147346490582,-0.350580908316224,
4.43937194476168));
#20929=CARTESIAN_POINT('Ctrl Pts',(9.16918930096864,-0.559175278946307,
3.94274891673689));
#20930=CARTESIAN_POINT('Ctrl Pts',(9.21690513703149,-0.254270386902387,
3.49870043939378));
#20931=CARTESIAN_POINT('Ctrl Pts',(9.26462097309432,0.284134913886797,3.51500306204057));
#20932=CARTESIAN_POINT('Ctrl Pts',(9.31233680915716,0.56161475127612,3.97668583545263));
#20933=CARTESIAN_POINT('Ctrl Pts',(9.36005264522,0.323355121014866,4.45977836490307));
#20934=CARTESIAN_POINT('Ctrl Pts',(9.40776848128284,-0.211846492332409,
4.52064934726353));
#20935=CARTESIAN_POINT('Ctrl Pts',(9.45548431734568,-0.552506212093558,
4.10340002281193));
#20936=CARTESIAN_POINT('Ctrl Pts',(9.50320015340851,-0.385790975888367,
3.59119686639829));
#20937=CARTESIAN_POINT('Ctrl Pts',(9.55091598947136,0.135202049632292,3.45440391781584));
#20938=CARTESIAN_POINT('Ctrl Pts',(9.59863182553417,0.532036952624682,3.81864024657791));
#20939=CARTESIAN_POINT('Ctrl Pts',(9.64634766159704,0.440294135581046,4.34942202748599));
#20940=CARTESIAN_POINT('Ctrl Pts',(9.69406349765985,-0.0557775609627595,
4.55932418400469));
#20941=CARTESIAN_POINT('Ctrl Pts',(9.74177933372271,-0.500627865026369,
4.25559033604309));
#20942=CARTESIAN_POINT('Ctrl Pts',(9.78949516978553,-0.485743897486414,
3.71714394973028));
#20943=CARTESIAN_POINT('Ctrl Pts',(9.83721100584839,-0.0247938347541151,
3.43844862667992));
#20944=CARTESIAN_POINT('Ctrl Pts',(9.88492684191122,0.458924787935076,3.67543457032792));
#20945=CARTESIAN_POINT('Ctrl Pts',(9.93264267797406,0.521205716397956,4.21047394212484));
#20946=CARTESIAN_POINT('Ctrl Pts',(9.98035851403688,0.104855415711801,4.55223185431066));
#20947=CARTESIAN_POINT('Ctrl Pts',(10.0280743500997,-0.407785226630454,
4.3868667575037));
#20948=CARTESIAN_POINT('Ctrl Pts',(10.0757901861625,-0.54595042077573,3.86623596457089));
#20949=CARTESIAN_POINT('Ctrl Pts',(10.1235060222254,-0.182760942995651,
3.46844274359687));
#20950=CARTESIAN_POINT('Ctrl Pts',(10.1712218582882,0.34826072087591,3.55878673023755));
#20951=CARTESIAN_POINT('Ctrl Pts',(10.2189376943511,0.559469206087141,4.05430365143988));
#20952=CARTESIAN_POINT('Ctrl Pts',(10.2666535304139,0.256908510808291,4.49995269395588));
#20953=CARTESIAN_POINT('Ctrl Pts',(10.3143693664768,-0.281575222991369,
4.4864874848512));
#20954=CARTESIAN_POINT('Ctrl Pts',(10.3620852025396,-0.561484096926345,
4.02627333283551));
#20955=CARTESIAN_POINT('Ctrl Pts',(10.4098010386024,-0.325773485110519,
3.5419319750098));
#20956=CARTESIAN_POINT('Ctrl Pts',(10.4575168746653,0.209099930751681,3.47824153281512));
#20957=CARTESIAN_POINT('Ctrl Pts',(10.5052327107281,0.55195366278862,3.89368991932227));
#20958=CARTESIAN_POINT('Ctrl Pts',(10.552948546791,0.387939853388008,4.40676448870664));
#20959=CARTESIAN_POINT('Ctrl Pts',(10.6006643828538,-0.13232509260073,4.54630096923553));
#20960=CARTESIAN_POINT('Ctrl Pts',(10.6483802189166,-0.531073869970951,
4.18416086379456));
#20961=CARTESIAN_POINT('Ctrl Pts',(10.6960960549795,-0.442129340924997,
3.6529030034519));
#20962=CARTESIAN_POINT('Ctrl Pts',(10.7438118910423,0.0528293649267388,
3.44038965581316));
#20963=CARTESIAN_POINT('Ctrl Pts',(10.7915277271051,0.499274052081986,3.74177509795313));
#20964=CARTESIAN_POINT('Ctrl Pts',(10.839243563168,0.487227694891584,4.28029244094358));
#20965=CARTESIAN_POINT('Ctrl Pts',(10.8869593992308,0.0277526485205102,
4.56141292256198));
#20966=CARTESIAN_POINT('Ctrl Pts',(10.9346752352937,-0.457208082016334,
4.32697927894352));
#20967=CARTESIAN_POINT('Ctrl Pts',(10.9823910713565,-0.522307595786967,
3.79227553224832));
#20968=CARTESIAN_POINT('Ctrl Pts',(11.0301069074193,-0.107764007611043,
3.44832836054127));
#20969=CARTESIAN_POINT('Ctrl Pts',(11.0778227434822,0.405740926916492,3.61098974390844));
#20970=CARTESIAN_POINT('Ctrl Pts',(11.125538579545,0.54664772512998,4.13088523113667));
#20971=CARTESIAN_POINT('Ctrl Pts',(11.1732544156078,0.185559506100192,4.53058679668394));
#20972=CARTESIAN_POINT('Ctrl Pts',(11.2209702516707,-0.345930862581405,
4.4430423427091));
#20973=CARTESIAN_POINT('Ctrl Pts',(11.2686860877335,-0.559747597323992,
3.94864528834179));
#20974=CARTESIAN_POINT('Ctrl Pts',(11.3164019237964,-0.259539500620097,
3.50140805588402));
#20975=CARTESIAN_POINT('Ctrl Pts',(11.3641177598592,0.279007713031768,3.51203547753114));
#20976=CARTESIAN_POINT('Ctrl Pts',(11.411833595922,0.561337850721073,3.97076822846069));
#20977=CARTESIAN_POINT('Ctrl Pts',(11.4595494319849,0.328182802800164,4.45634496498341));
#20978=CARTESIAN_POINT('Ctrl Pts',(11.5072652680477,-0.206347562673641,
4.52285309839201));
#20979=CARTESIAN_POINT('Ctrl Pts',(11.5549811041106,-0.551385786278872,
4.10921718641821));
#20980=CARTESIAN_POINT('Ctrl Pts',(11.6026969401734,-0.390077958183356,
3.59528545163414));
#20981=CARTESIAN_POINT('Ctrl Pts',(11.6504127762362,0.129444461032819,3.45300931394821));
#20982=CARTESIAN_POINT('Ctrl Pts',(11.6981286122991,0.530096039923511,3.8130431397972));
#20983=CARTESIAN_POINT('Ctrl Pts',(11.7458444483619,0.443952268776438,4.34476232707146));
#20984=CARTESIAN_POINT('Ctrl Pts',(11.7935602844247,-0.0498797018717475,
4.55988096454574));
#20985=CARTESIAN_POINT('Ctrl Pts',(11.8412761204876,-0.497906374793238,
4.26085229740167));
#20986=CARTESIAN_POINT('Ctrl Pts',(11.8889919565504,-0.48869796246776,3.72227895182515));
#20987=CARTESIAN_POINT('Ctrl Pts',(11.9367077926133,-0.0307106916234339,
3.43874111807518));
#20988=CARTESIAN_POINT('Ctrl Pts',(11.9844236286761,0.455478679883424,3.67061595167475));
#20989=CARTESIAN_POINT('Ctrl Pts',(12.0321394647389,0.523394971212992,4.20496922507643));
#20990=CARTESIAN_POINT('Ctrl Pts',(12.0798553008018,0.110669607010866,4.5510961052335));
#20991=CARTESIAN_POINT('Ctrl Pts',(12.1275711368646,-0.403685360180124,
4.39114295225112));
#20992=CARTESIAN_POINT('Ctrl Pts',(12.1752869729274,-0.547329849620031,
3.8719972077086));
#20993=CARTESIAN_POINT('Ctrl Pts',(12.2230028089903,-0.188352916401613,
3.4703983969034));
#20994=CARTESIAN_POINT('Ctrl Pts',(12.2707186450531,0.34359139813055,3.55514088718992));
#20995=CARTESIAN_POINT('Ctrl Pts',(12.318434481116,0.560010444926212,4.04840434580723));
#20996=CARTESIAN_POINT('Ctrl Pts',(12.3661503171788,0.262163283277844,4.49721734887317));
#20997=CARTESIAN_POINT('Ctrl Pts',(12.4138661532417,-0.276432455305192,
4.48942800979656));
#20998=CARTESIAN_POINT('Ctrl Pts',(12.4615819893045,-0.561176016721412,
4.03218939850585));
#20999=CARTESIAN_POINT('Ctrl Pts',(12.5092978253673,-0.330583007179444,
3.54539076726965));
#21000=CARTESIAN_POINT('Ctrl Pts',(12.5570136614301,0.203589464528802,3.47606678951191));
#21001=CARTESIAN_POINT('Ctrl Pts',(12.604729497493,0.550802598333678,3.88787874069406));
#21002=CARTESIAN_POINT('Ctrl Pts',(12.6524453335558,0.392205230901379,4.40265336950419));
#21003=CARTESIAN_POINT('Ctrl Pts',(12.7001611696187,-0.126560234920843,
4.54766521348015));
#21004=CARTESIAN_POINT('Ctrl Pts',(12.7478770056815,-0.529103489635726,
4.18974766500481));
#21005=CARTESIAN_POINT('Ctrl Pts',(12.7955928417443,-0.44576286851447,3.65758191611243));
#21006=CARTESIAN_POINT('Ctrl Pts',(12.8433086778072,0.0469286537069902,
3.43986396243348));
#21007=CARTESIAN_POINT('Ctrl Pts',(12.89102451387,0.496524871139168,3.73652755085263));
#21008=CARTESIAN_POINT('Ctrl Pts',(12.9387403499328,0.490154659387074,4.27514194336855));
#21009=CARTESIAN_POINT('Ctrl Pts',(12.9864561859957,0.0336678819209607,
4.56108925568614));
#21010=CARTESIAN_POINT('Ctrl Pts',(13.0341720220585,-0.45373662956012,4.33177967103923));
#21011=CARTESIAN_POINT('Ctrl Pts',(13.0818878581214,-0.524467812480695,
3.79779170939055));
#21012=CARTESIAN_POINT('Ctrl Pts',(13.1296036941842,-0.113572133225654,
3.44949473238301));
#21013=CARTESIAN_POINT('Ctrl Pts',(13.177319530247,0.401618583502394,3.60673521324049));
#21014=CARTESIAN_POINT('Ctrl Pts',(13.2250353663099,0.547996775303968,4.12511679893576));
#21015=CARTESIAN_POINT('Ctrl Pts',(13.2727512023727,0.191141096329688,4.52860170299893));
#21016=CARTESIAN_POINT('Ctrl Pts',(13.3204670384356,-0.341242392487953,
4.4466635296155));
#21017=CARTESIAN_POINT('Ctrl Pts',(13.3681828744984,-0.560257741594785,
3.95454736418435));
#21018=CARTESIAN_POINT('Ctrl Pts',(13.4158987105612,-0.264779785921688,
3.5041710536014));
#21019=CARTESIAN_POINT('Ctrl Pts',(13.4636145466241,0.273849521323983,3.50912209380529));
#21020=CARTESIAN_POINT('Ctrl Pts',(13.5113303826869,0.560998599421335,3.96485386839523));
#21021=CARTESIAN_POINT('Ctrl Pts',(13.5590462187498,0.332974031597074,4.45286087643057));
#21022=CARTESIAN_POINT('Ctrl Pts',(13.6067620548126,-0.200825712906817,
4.52499877347948));
#21023=CARTESIAN_POINT('Ctrl Pts',(13.6544778908754,-0.550204115147588,
4.11502221869768));
#21024=CARTESIAN_POINT('Ctrl Pts',(13.7021937269383,-0.394321612469819,
3.5994189906415));
#21025=CARTESIAN_POINT('Ctrl Pts',(13.7499095630011,0.123672494356884,3.45167546721031));
#21026=CARTESIAN_POINT('Ctrl Pts',(13.7976253990639,0.528096246669736,3.80746679929733));
#21027=CARTESIAN_POINT('Ctrl Pts',(13.8453412351268,0.44756108986054,4.34006433209368));
#21028=CARTESIAN_POINT('Ctrl Pts',(13.8930570711896,-0.0439763023801491,
4.56037555616609));
#21029=CARTESIAN_POINT('Ctrl Pts',(13.9407729072525,-0.495129579482757,
4.26608528452492));
#21030=CARTESIAN_POINT('Ctrl Pts',(13.9884887433153,-0.491597745198497,
3.72744480185615));
#21031=CARTESIAN_POINT('Ctrl Pts',(14.0362045793781,-0.0366241372948624,
3.43909595144367));
#21032=CARTESIAN_POINT('Ctrl Pts',(14.083920415441,0.451981979421435,3.66583391943861));
#21033=CARTESIAN_POINT('Ctrl Pts',(14.1316362515038,0.525526089798339,4.19944174101915));
#21034=CARTESIAN_POINT('Ctrl Pts',(14.1793520875667,0.11647150565515,4.54989914301615));
#21035=CARTESIAN_POINT('Ctrl Pts',(14.2270679236295,-0.399540654275635,
4.39537570069553));
#21036=CARTESIAN_POINT('Ctrl Pts',(14.2747837596924,-0.548648483661927,
3.87777266878906));
#21037=CARTESIAN_POINT('Ctrl Pts',(14.3224995957551,-0.193923968459428,
3.47241287584284));
#21038=CARTESIAN_POINT('Ctrl Pts',(14.370215431818,0.338883910883161,3.5515444569815));
#21039=CARTESIAN_POINT('Ctrl Pts',(14.4179312678808,0.560489480462528,4.04249966364955));
#21040=CARTESIAN_POINT('Ctrl Pts',(14.4656471039437,0.267388935893957,4.49442677524682));
#21041=CARTESIAN_POINT('Ctrl Pts',(14.5133629400065,-0.271258982813659,
4.49231417140114));
#21042=CARTESIAN_POINT('Ctrl Pts',(14.5610787760694,-0.560805603747543,
4.03810188873054));
#21043=CARTESIAN_POINT('Ctrl Pts',(14.6087946121322,-0.335355809656676,
3.54890005536578));
#21044=CARTESIAN_POINT('Ctrl Pts',(14.656510448195,0.198056384554314,3.47395024222346));
#21045=CARTESIAN_POINT('Ctrl Pts',(14.7042262842579,0.549590353339887,3.88208001596329));
#21046=CARTESIAN_POINT('Ctrl Pts',(14.7519421203207,0.396427044118869,4.3984975254762));
#21047=CARTESIAN_POINT('Ctrl Pts',(14.7996579563836,-0.120781319530639,
4.54896862567174));
#21048=CARTESIAN_POINT('Ctrl Pts',(14.8473737924464,-0.527074338995675,
4.19531338994486));
#21049=CARTESIAN_POINT('Ctrl Pts',(14.8950896285092,-0.449346882879826,
3.66229886294881));
#21050=CARTESIAN_POINT('Ctrl Pts',(14.9428054645721,0.041022729875082,3.43940048630678));
#21051=CARTESIAN_POINT('Ctrl Pts',(14.9905213006349,0.493720538569869,3.73130926902151));
#21052=CARTESIAN_POINT('Ctrl Pts',(15.0382371366977,0.493027179828974,4.2699608843321));
#21053=CARTESIAN_POINT('Ctrl Pts',(15.0859529727606,0.0395793756528551,
4.56070326567839));
#21054=CARTESIAN_POINT('Ctrl Pts',(15.1336688088234,-0.450214778192253,
4.33654321062351));
#21055=CARTESIAN_POINT('Ctrl Pts',(15.1813846448863,-0.526569773778615,
3.80333034687015));
#21056=CARTESIAN_POINT('Ctrl Pts',(15.2291004809491,-0.119367643786657,
3.45072225173751));
#21057=CARTESIAN_POINT('Ctrl Pts',(15.2768163170119,0.397451630201876,3.60252436455885));
#21058=CARTESIAN_POINT('Ctrl Pts',(15.3245321530748,0.549284956596614,4.11933446935456));
#21059=CARTESIAN_POINT('Ctrl Pts',(15.3722479891376,0.196701455513243,4.52655789474516));
#21060=CARTESIAN_POINT('Ctrl Pts',(15.4199638252005,-0.336516018808871,
4.45023510325662));
#21061=CARTESIAN_POINT('Ctrl Pts',(15.4676796612633,-0.560705655094284,
3.96045448869));
#21062=CARTESIAN_POINT('Ctrl Pts',(15.5153954973261,-0.269990660741143,
3.50698912564524));
#21063=CARTESIAN_POINT('Ctrl Pts',(15.5631113333889,0.268660911710894,3.50626323446785));
#21064=CARTESIAN_POINT('Ctrl Pts',(15.6108271694518,0.560597035059331,3.95894341219528));
#21065=CARTESIAN_POINT('Ctrl Pts',(15.6585430055146,0.337728275218647,4.44932648624059));
#21066=CARTESIAN_POINT('Ctrl Pts',(15.7062588415775,-0.1952815563728,4.52708613419449));
#21067=CARTESIAN_POINT('Ctrl Pts',(15.7539746776403,-0.548961329954127,
4.12081447485494));
#21068=CARTESIAN_POINT('Ctrl Pts',(15.8016905137031,-0.398521467382777,
3.60359702428645));
#21069=CARTESIAN_POINT('Ctrl Pts',(15.849406349766,0.117886790727162,3.4504025257595));
#21070=CARTESIAN_POINT('Ctrl Pts',(15.8971221858288,0.526037794990907,3.80191184447176));
#21071=CARTESIAN_POINT('Ctrl Pts',(15.9448380218916,0.451120197982628,4.33532856438364));
#21072=CARTESIAN_POINT('Ctrl Pts',(15.9925538579545,-0.0380680182095728,
4.56080790392885));
#21073=CARTESIAN_POINT('Ctrl Pts',(16.0402696940173,-0.492297787528177,
4.27128871615743));
#21074=CARTESIAN_POINT('Ctrl Pts',(16.0879855300802,-0.494442923584513,
3.73264092602517));
#21075=CARTESIAN_POINT('Ctrl Pts',(16.135701366143,-0.0425335149309099,
3.43951308737216));
#21076=CARTESIAN_POINT('Ctrl Pts',(16.1834172022058,0.448435074945997,3.66108900478495));
#21077=CARTESIAN_POINT('Ctrl Pts',(16.2311330382687,0.52759883543946,4.19389210391969));
#21078=CARTESIAN_POINT('Ctrl Pts',(16.2788488743315,0.122260467197297,4.54864110061148));
#21079=CARTESIAN_POINT('Ctrl Pts',(16.3265647103944,-0.395351569291248,
4.39956453268331));
#21080=CARTESIAN_POINT('Ctrl Pts',(16.3742805464572,-0.549906176433804,
3.88356170630145));
#21081=CARTESIAN_POINT('Ctrl Pts',(16.42199638252,-0.199473480363076,3.47448595665642));
#21082=CARTESIAN_POINT('Ctrl Pts',(16.4697122185829,0.334138782019088,3.54799783908671));
#21083=CARTESIAN_POINT('Ctrl Pts',(16.5174280546457,0.560906259487099,4.0365902608309));
#21084=CARTESIAN_POINT('Ctrl Pts',(16.5651438907085,0.272584888215931,4.49158128304055));
#21085=CARTESIAN_POINT('Ctrl Pts',(16.6128597267714,-0.26605538016154,4.49514564908375));
#21086=CARTESIAN_POINT('Ctrl Pts',(16.6605755628342,-0.560372899148451,
4.04401014677825));
#21087=CARTESIAN_POINT('Ctrl Pts',(16.7082913988971,-0.340091362401967,
3.55245944950311));
#21088=CARTESIAN_POINT('Ctrl Pts',(16.7560072349599,0.19250130541649,3.4718921260458));
#21089=CARTESIAN_POINT('Ctrl Pts',(16.8037230710227,0.548317062457662,3.87629438922476));
#21090=CARTESIAN_POINT('Ctrl Pts',(16.8514389070856,0.400604824101502,4.39429741823411));
#21091=CARTESIAN_POINT('Ctrl Pts',(16.8991547431484,-0.114988988324618,
4.55021106103346));
#21092=CARTESIAN_POINT('Ctrl Pts',(16.9468705792113,-0.524986643439221,
4.20085742040038));
#21093=CARTESIAN_POINT('Ctrl Pts',(16.9945864152741,-0.45288098592576,3.66705332002498));
#21094=CARTESIAN_POINT('Ctrl Pts',(17.0423022513369,0.0351122494330066,
3.4389992789138));
#21095=CARTESIAN_POINT('Ctrl Pts',(17.0900180873998,0.490861365866046,3.72612083208173));
#21096=CARTESIAN_POINT('Ctrl Pts',(17.1377339234626,0.49584493715134,4.26474983932169));
#21097=CARTESIAN_POINT('Ctrl Pts',(17.1854497595254,0.0454864730955262,
4.56025499541263));
#21098=CARTESIAN_POINT('Ctrl Pts',(17.2331655955883,-0.446642919103261,
4.34126936858499));
#21099=CARTESIAN_POINT('Ctrl Pts',(17.2808814316511,-0.528613246204851,
3.80889082948154));
#21100=CARTESIAN_POINT('Ctrl Pts',(17.328597267714,-0.125149895556227,3.45201078225777));
#21101=CARTESIAN_POINT('Ctrl Pts',(17.3763131037768,0.393240529860342,3.59835766558462));
#21102=CARTESIAN_POINT('Ctrl Pts',(17.4240289398397,0.55051212592285,4.1135388846668));
#21103=CARTESIAN_POINT('Ctrl Pts',(17.4717447759024,0.202239966032548,4.52445559893916));
#21104=CARTESIAN_POINT('Ctrl Pts',(17.5194606119653,-0.331752266527324,
4.45375666691904));
#21105=CARTESIAN_POINT('Ctrl Pts',(17.5671764480281,-0.561091288070378,
3.96636600572338));
#21106=CARTESIAN_POINT('Ctrl Pts',(17.614892284091,-0.275171546279217,3.50986195899749));
#21107=CARTESIAN_POINT('Ctrl Pts',(17.6626081201538,0.263442460518632,3.50345921706735));
#21108=CARTESIAN_POINT('Ctrl Pts',(17.7103239562167,0.560133202238927,3.95303751636628));
#21109=CARTESIAN_POINT('Ctrl Pts',(17.7580397922795,0.342445005586054,4.44574218699675));
#21110=CARTESIAN_POINT('Ctrl Pts',(17.8057556283423,-0.189715708890181,
4.52911494868296));
#21111=CARTESIAN_POINT('Ctrl Pts',(17.8534714644052,-0.547657568741173,
4.12659331151364));
#21112=CARTESIAN_POINT('Ctrl Pts',(17.901187300468,-0.402677056422281,3.60781908849286));
#21113=CARTESIAN_POINT('Ctrl Pts',(17.9489031365308,0.112087992792125,3.44919063098808));
#21114=CARTESIAN_POINT('Ctrl Pts',(17.9966189725937,0.523920913530056,3.79637889233847));
#21115=CARTESIAN_POINT('Ctrl Pts',(18.0443348086565,0.454629197813879,4.33055554996792));
#21116=CARTESIAN_POINT('Ctrl Pts',(18.0920506447194,-0.0321555056241734,
4.56117795981091));
#21117=CARTESIAN_POINT('Ctrl Pts',(18.1397664807822,-0.489411313471489,
4.27646201432672));
#21118=CARTESIAN_POINT('Ctrl Pts',(18.1874823168451,-0.497233181596917,
3.73786674717144));
#21119=CARTESIAN_POINT('Ctrl Pts',(18.2351981529079,-0.0484381681459794,
3.43999247952716));
#21120=CARTESIAN_POINT('Ctrl Pts',(18.2829139889707,0.444838360430441,3.65638173475637));
#21121=CARTESIAN_POINT('Ctrl Pts',(18.3306298250336,0.529612977905601,4.18832093020544));
#21122=CARTESIAN_POINT('Ctrl Pts',(18.3783456610964,0.128035848626906,4.54732211775687));
#21123=CARTESIAN_POINT('Ctrl Pts',(18.4260614971592,-0.391118570530631,
4.40370898293889));
#21124=CARTESIAN_POINT('Ctrl Pts',(18.4737773332221,-0.551102788237131,
3.88936367722697));
#21125=CARTESIAN_POINT('Ctrl Pts',(18.5214931692849,-0.205000835699102,
3.47661740907615));
#21126=CARTESIAN_POINT('Ctrl Pts',(18.5692090053478,0.329356538604741,3.54450142744705));
#21127=CARTESIAN_POINT('Ctrl Pts',(18.6169248414106,0.561260735706054,4.03067679373969));
#21128=CARTESIAN_POINT('Ctrl Pts',(18.6646406774734,0.2777505631021,4.48868118831814));
#21129=CARTESIAN_POINT('Ctrl Pts',(18.7123565135363,-0.260822225340423,
4.49792212833724));
#21130=CARTESIAN_POINT('Ctrl Pts',(18.7600723495991,-0.559877950986752,
4.04991351638789));
#21131=CARTESIAN_POINT('Ctrl Pts',(18.8077881856619,-0.344789139412875,
3.55606855432066));
#21132=CARTESIAN_POINT('Ctrl Pts',(18.8555040217248,0.186924844147682,3.46989266958543));
#21133=CARTESIAN_POINT('Ctrl Pts',(18.9032198577876,0.546982867117114,3.87052250311704));
#21134=CARTESIAN_POINT('Ctrl Pts',(18.9509356938504,0.404738106803207,4.39005351430856));
#21135=CARTESIAN_POINT('Ctrl Pts',(18.9986515299133,-0.109183884691052,
4.55139238155646));
#21136=CARTESIAN_POINT('Ctrl Pts',(19.0463673659761,-0.522840634850846,
4.20637914057629));
#21137=CARTESIAN_POINT('Ctrl Pts',(19.094083202039,-0.456364785113784,3.67184475922049));
#21138=CARTESIAN_POINT('Ctrl Pts',(19.1417990381018,0.029197868913272,3.43866038485254));
#21139=CARTESIAN_POINT('Ctrl Pts',(19.1895148741647,0.487947670564988,3.72096281627648));
#21140=CARTESIAN_POINT('Ctrl Pts',(19.2372307102275,0.498607618457993,4.25950938727589));
#21141=CARTESIAN_POINT('Ctrl Pts',(19.2849465462903,0.0513885179525073,
4.55974449445321));
#21142=CARTESIAN_POINT('Ctrl Pts',(19.3326623823531,-0.44302144872845,4.34595762039384));
#21143=CARTESIAN_POINT('Ctrl Pts',(19.380378218416,-0.530598003365269,3.81447253878192));
#21144=CARTESIAN_POINT('Ctrl Pts',(19.4280940544788,-0.130918245164485,
3.45336018235082));
#21145=CARTESIAN_POINT('Ctrl Pts',(19.4758098905417,0.38898574814073,3.59423557624425));
#21146=CARTESIAN_POINT('Ctrl Pts',(19.5235257266045,0.551678150913516,4.10773069407674));
#21147=CARTESIAN_POINT('Ctrl Pts',(19.5712415626673,0.207756005258534,4.52229503878775));
#21148=CARTESIAN_POINT('Ctrl Pts',(19.6189573987302,-0.326951650734615,
4.4572278489044));
#21149=CARTESIAN_POINT('Ctrl Pts',(19.666673234793,-0.561414624206118,3.9722812219163));
#21150=CARTESIAN_POINT('Ctrl Pts',(19.7143890708559,-0.280321816997631,
3.51278930393937));
#21151=CARTESIAN_POINT('Ctrl Pts',(19.7621049069187,0.258194652845487,3.5007102220535));
#21152=CARTESIAN_POINT('Ctrl Pts',(19.8098207429815,0.559607330995945,3.94713708427543));
#21153=CARTESIAN_POINT('Ctrl Pts',(19.8575365790444,0.347123361713752,4.44210790974427));
#21154=CARTESIAN_POINT('Ctrl Pts',(19.9052524151072,-0.184128152223511,
4.53108587353909));
#21155=CARTESIAN_POINT('Ctrl Pts',(19.9529682511701,-0.546294178096705,
4.13235642149579));
#21156=CARTESIAN_POINT('Ctrl Pts',(20.0006840872329,-0.406785648814185,
3.61208785870539));
#21157=CARTESIAN_POINT('Ctrl Pts',(20.0483999232957,0.106272459957556,3.44803398021027));
#21158=CARTESIAN_POINT('Ctrl Pts',(20.0961157593586,0.5217539278249,3.7908797683689));
#21159=CARTESIAN_POINT('Ctrl Pts',(20.1438315954214,0.458072423058868,4.32572464996293));
#21160=CARTESIAN_POINT('Ctrl Pts',(20.1915474314842,-0.0262105744965466,
4.56152565902554));
#21161=CARTESIAN_POINT('Ctrl Pts',(20.2392632675471,-0.486524960252488,
4.28152908133109));
#21162=CARTESIAN_POINT('Ctrl Pts',(20.2869791036099,-0.499865224545849,
3.74326461201656));
#21163=CARTESIAN_POINT('Ctrl Pts',(20.3346949396728,-0.0545328049175168,
3.440261547834));
#21164=CARTESIAN_POINT('Ctrl Pts',(20.3824107757356,0.441568512678419,3.6522489094147));
#21165=CARTESIAN_POINT('Ctrl Pts',(20.4221739724547,0.515928418030698,4.09332268501583));
#21166=CARTESIAN_POINT('Ctrl Pts',(20.4539845298298,0.333108474939506,4.36566768059473));
#21167=CARTESIAN_POINT('Ctrl Pts',(20.4778424478613,0.118510552090848,4.48142006140068));
#21168=CARTESIAN_POINT('Ctrl Pts',(20.5017003658927,-0.127372553428812,
4.47887124859312));
#21169=CARTESIAN_POINT('Ctrl Pts',(20.5255582839241,-0.340862259689409,
4.35954554232165));
#21170=CARTESIAN_POINT('Ctrl Pts',(20.5494162019555,-0.471665647836603,
4.15213005589169));
#21171=CARTESIAN_POINT('Ctrl Pts',(20.5732741199869,-0.486782001098211,
3.90760543082941));
#21172=CARTESIAN_POINT('Ctrl Pts',(20.5971320380184,-0.38305332993788,3.68562568155832));
#21173=CARTESIAN_POINT('Ctrl Pts',(20.6209899560498,-0.185558943137764,
3.54054450025879));
#21174=CARTESIAN_POINT('Ctrl Pts',(20.6448478740812,0.0572573647513246,
3.50779920733485));
#21175=CARTESIAN_POINT('Ctrl Pts',(20.6687057921126,0.28610038304352,3.59541756340761));
#21176=CARTESIAN_POINT('Ctrl Pts',(20.6925637101441,0.444969396676924,3.78196356026503));
#21177=CARTESIAN_POINT('Ctrl Pts',(20.7164216281754,0.495039040219165,4.02182741068269));
#21178=CARTESIAN_POINT('Ctrl Pts',(20.7402795462069,0.424054039808096,4.25635280284423));
#21179=CARTESIAN_POINT('Ctrl Pts',(20.7641374642383,0.249378454468877,4.42819351412177));
#21180=CARTESIAN_POINT('Ctrl Pts',(20.7879953822697,0.0137218901755031,
4.49532894963167));
#21181=CARTESIAN_POINT('Ctrl Pts',(20.8118533003011,-0.22528943893053,4.44134312218709));
#21182=CARTESIAN_POINT('Ctrl Pts',(20.8357112183326,-0.409211687104306,
4.27943679589328));
#21183=CARTESIAN_POINT('Ctrl Pts',(20.859569136364,-0.493070359673604,4.04920060553547));
#21184=CARTESIAN_POINT('Ctrl Pts',(20.8834270543954,-0.456359989112496,
3.80693350349834));
#21185=CARTESIAN_POINT('Ctrl Pts',(20.9072849724268,-0.308057122141145,
3.61187643128937));
#21186=CARTESIAN_POINT('Ctrl Pts',(20.9311428904583,-0.0844259229598539,
3.51172613733272));
#21187=CARTESIAN_POINT('Ctrl Pts',(20.9550008084896,0.159849727585384,3.53097210659131));
#21188=CARTESIAN_POINT('Ctrl Pts',(20.9788587265211,0.365037758375503,3.66490817000854));
#21189=CARTESIAN_POINT('Ctrl Pts',(21.0027166445525,0.480964117596,3.88078331455297));
#21190=CARTESIAN_POINT('Ctrl Pts',(21.026574562584,0.479281646861755,4.12581018556955));
#21191=CARTESIAN_POINT('Ctrl Pts',(21.0504324806153,0.360401759160676,4.34007303948752));
#21192=CARTESIAN_POINT('Ctrl Pts',(21.0742903986468,0.153393823636192,4.47117877170218));
#21193=CARTESIAN_POINT('Ctrl Pts',(21.0981483166782,-0.0911230798336762,
4.48706845966041));
#21194=CARTESIAN_POINT('Ctrl Pts',(21.1220062347096,-0.313357908298923,
4.38385664171252));
#21195=CARTESIAN_POINT('Ctrl Pts',(21.145864152741,-0.458968192403581,4.18678141884249));
#21196=CARTESIAN_POINT('Ctrl Pts',(21.1697220707724,-0.492348251467217,
3.94403305123036));
#21197=CARTESIAN_POINT('Ctrl Pts',(21.1935799888039,-0.405335751726616,
3.71497012710753));
#21198=CARTESIAN_POINT('Ctrl Pts',(21.2174379068353,-0.21920761957706,3.55560477096155));
#21199=CARTESIAN_POINT('Ctrl Pts',(21.2412958248667,0.0205227466613194,
3.50490615340017));
#21200=CARTESIAN_POINT('Ctrl Pts',(21.2651537428981,0.255234742309135,3.57527146741714));
#21201=CARTESIAN_POINT('Ctrl Pts',(21.2890116609295,0.427534891009427,3.74949447702405));
#21202=CARTESIAN_POINT('Ctrl Pts',(21.312869578961,0.495291113040325,3.98497291063177));
#21203=CARTESIAN_POINT('Ctrl Pts',(21.3367274969923,0.441935166474334,4.22412587691986));
#21204=CARTESIAN_POINT('Ctrl Pts',(21.3605854150238,0.280514033632862,4.40847396123464));
#21205=CARTESIAN_POINT('Ctrl Pts',(21.3844433330552,0.0504995785194436,
4.49293903542029));
#21206=CARTESIAN_POINT('Ctrl Pts',(21.4083012510867,-0.191863399122956,
4.45686708805594));
#21207=CARTESIAN_POINT('Ctrl Pts',(21.432159169118,-0.387310549425693,4.3090786928523));
#21208=CARTESIAN_POINT('Ctrl Pts',(21.4560170871495,-0.488049720266331,
4.08571213811173));
#21209=CARTESIAN_POINT('Ctrl Pts',(21.4798750051809,-0.469447440294381,
3.84138663085107));
#21210=CARTESIAN_POINT('Ctrl Pts',(21.5037329232123,-0.336052473678932,
3.63584641288874));
#21211=CARTESIAN_POINT('Ctrl Pts',(21.5275908412437,-0.120483523363382,
3.51935166631968));
#21212=CARTESIAN_POINT('Ctrl Pts',(21.5514487592752,0.124546930319796,3.5203885299332));
#21213=CARTESIAN_POINT('Ctrl Pts',(21.5753066773065,0.339122266949511,3.63870346233219));
#21214=CARTESIAN_POINT('Ctrl Pts',(21.599164595338,0.470772971804989,3.84536523971104));
#21215=CARTESIAN_POINT('Ctrl Pts',(21.6230225133694,0.487306861455871,4.08983942814686));
#21216=CARTESIAN_POINT('Ctrl Pts',(21.6468804314008,0.384680949508402,4.31234542922385));
#21217=CARTESIAN_POINT('Ctrl Pts',(21.6707383494323,0.187990066907445,4.45847446473699));
#21218=CARTESIAN_POINT('Ctrl Pts',(21.6945962674636,-0.0546695077989956,
4.49249400502822));
#21219=CARTESIAN_POINT('Ctrl Pts',(21.7184541854951,-0.283960898681086,
4.40608534582272));
#21220=CARTESIAN_POINT('Ctrl Pts',(21.7423121035264,-0.443816114896065,
4.22037775802082));
#21221=CARTESIAN_POINT('Ctrl Pts',(21.766170021558,-0.495146201710716,3.98078180541326));
#21222=CARTESIAN_POINT('Ctrl Pts',(21.7900279395893,-0.425399554695369,
3.74588522487523));
#21223=CARTESIAN_POINT('Ctrl Pts',(21.8138858576208,-0.25163112890579,3.57312662880273));
#21224=CARTESIAN_POINT('Ctrl Pts',(21.8377437756521,-0.0163320378044167,
3.50475019978512));
#21225=CARTESIAN_POINT('Ctrl Pts',(21.8616016936836,0.222960681415914,3.55747583725374));
#21226=CARTESIAN_POINT('Ctrl Pts',(21.885459611715,0.407733440703041,3.71841068663001));
#21227=CARTESIAN_POINT('Ctrl Pts',(21.9093175297464,0.492804267302335,3.94820179346412));
#21228=CARTESIAN_POINT('Ctrl Pts',(21.9331754477779,0.457371026827486,4.19065897275109));
#21229=CARTESIAN_POINT('Ctrl Pts',(21.9570333658092,0.310098111756678,4.38649483975425));
#21230=CARTESIAN_POINT('Ctrl Pts',(21.9808912838407,0.0869977614584207,
4.48782219052945));
#21231=CARTESIAN_POINT('Ctrl Pts',(22.0047492018721,-0.15737591128791,4.46986372771052));
#21232=CARTESIAN_POINT('Ctrl Pts',(22.0286071199035,-0.363266886890503,
4.33701078463543));
#21233=CARTESIAN_POINT('Ctrl Pts',(22.0524650379349,-0.480329213457224,
4.12174952472744));
#21234=CARTESIAN_POINT('Ctrl Pts',(22.0763229559664,-0.479937963428243,
3.87671718963328));
#21235=CARTESIAN_POINT('Ctrl Pts',(22.1001808739978,-0.362188808094022,
3.66183085982978));
#21236=CARTESIAN_POINT('Ctrl Pts',(22.1240387920292,-0.155874623354616,
3.529636096341));
#21237=CARTESIAN_POINT('Ctrl Pts',(22.1478967100606,0.0885551527323001,
3.51245811975107));
#21238=CARTESIAN_POINT('Ctrl Pts',(22.1717546280921,0.311330781786364,3.61449741325855));
#21239=CARTESIAN_POINT('Ctrl Pts',(22.1956125461234,0.457977554205651,3.81080259009947));
#21240=CARTESIAN_POINT('Ctrl Pts',(22.2194704641549,0.492636339578261,4.05337168730347));
#21241=CARTESIAN_POINT('Ctrl Pts',(22.2433283821863,0.406832120751761,4.28288995313029));
#21242=CARTESIAN_POINT('Ctrl Pts',(22.2671863002177,0.22154636656941,4.44323391967918));
#21243=CARTESIAN_POINT('Ctrl Pts',(22.2910442182491,-0.0179135091400202,
4.49519511936025));
#21244=CARTESIAN_POINT('Ctrl Pts',(22.3149021362805,-0.2529930437236,4.42606762362056));
#21245=CARTESIAN_POINT('Ctrl Pts',(22.338760054312,-0.426208888077552,4.25275498785448));
#21246=CARTESIAN_POINT('Ctrl Pts',(22.3626179723434,-0.495205048933098,
4.01763687303198));
#21247=CARTESIAN_POINT('Ctrl Pts',(22.3864758903748,-0.443110087468167,
3.77820606161377));
#21248=CARTESIAN_POINT('Ctrl Pts',(22.4103338084062,-0.282662637164788,
3.59300991103726));
#21249=CARTESIAN_POINT('Ctrl Pts',(22.4341917264377,-0.0530964769854286,
3.50733392083031));
#21250=CARTESIAN_POINT('Ctrl Pts',(22.458049644469,0.189453226607198,3.5421282117862));
#21251=CARTESIAN_POINT('Ctrl Pts',(22.4819075625005,0.385676439696491,3.6888846179772));
#21252=CARTESIAN_POINT('Ctrl Pts',(22.5057654805319,0.487591287867653,3.9117172269821));
#21253=CARTESIAN_POINT('Ctrl Pts',(22.5296233985634,0.470276727405835,4.15613734610506));
#21254=CARTESIAN_POINT('Ctrl Pts',(22.5534813165947,0.337966804695391,4.36237769267677));
#21255=CARTESIAN_POINT('Ctrl Pts',(22.5773392346262,0.123014588878675,4.48000670597833));
#21256=CARTESIAN_POINT('Ctrl Pts',(22.6011971526576,-0.122017660845505,
4.48026122441149));
#21257=CARTESIAN_POINT('Ctrl Pts',(22.625055070689,-0.337213993725473,4.36307837627545));
#21258=CARTESIAN_POINT('Ctrl Pts',(22.6489129887204,-0.469950950795418,
4.15711375897153));
#21259=CARTESIAN_POINT('Ctrl Pts',(22.6727709067518,-0.487774683880463,
3.912729067726));
#21260=CARTESIAN_POINT('Ctrl Pts',(22.6966288247832,-0.386319338946922,
3.6896872918462));
#21261=CARTESIAN_POINT('Ctrl Pts',(22.7204867428147,-0.190407614498503,
3.54252014522276));
#21262=CARTESIAN_POINT('Ctrl Pts',(22.7443446608461,0.0520814161336476,
3.50722927763546));
#21263=CARTESIAN_POINT('Ctrl Pts',(22.7682025788775,0.281801791424649,3.59241522467272));
#21264=CARTESIAN_POINT('Ctrl Pts',(22.7920604969089,0.442679857002608,3.77730419914427));
#21265=CARTESIAN_POINT('Ctrl Pts',(22.8079657755965,0.477669651496365,3.93681187972983));
#21266=CARTESIAN_POINT('Ctrl Pts',(22.8159184149403,0.475016281724327,4.01593044384941));
#21267=CARTESIAN_POINT('Ctrl Pts',(3.98408158505964,0.229225853138217,4.48306385360099));
#21268=CARTESIAN_POINT('Ctrl Pts',(3.99203422440344,0.148766887950233,4.52124364039387));
#21269=CARTESIAN_POINT('Ctrl Pts',(4.00793950309106,-0.0315132651739855,
4.55658776856145));
#21270=CARTESIAN_POINT('Ctrl Pts',(4.03179742112247,-0.29437836981663,4.47338935048851));
#21271=CARTESIAN_POINT('Ctrl Pts',(4.0556553391539,-0.485191777607318,4.27448557757091));
#21272=CARTESIAN_POINT('Ctrl Pts',(4.07951325718531,-0.557397168683185,
4.00843674174317));
#21273=CARTESIAN_POINT('Ctrl Pts',(4.10337117521674,-0.493285636019562,
3.74033843218029));
#21274=CARTESIAN_POINT('Ctrl Pts',(4.12722909324815,-0.308561908987092,
3.53572729771651));
#21275=CARTESIAN_POINT('Ctrl Pts',(4.15108701127957,-0.0483813190761145,
3.44464727048097));
#21276=CARTESIAN_POINT('Ctrl Pts',(4.17494492931099,0.223627135909104,3.48936410886239));
#21277=CARTESIAN_POINT('Ctrl Pts',(4.19880284734241,0.440954086798485,3.65894639349553));
#21278=CARTESIAN_POINT('Ctrl Pts',(4.22266076537383,0.55045499896491,3.91192501290154));
#21279=CARTESIAN_POINT('Ctrl Pts',(4.24651868340524,0.525355068663259,4.18644066347397));
#21280=CARTESIAN_POINT('Ctrl Pts',(4.27037660143667,0.371791302444591,4.41536633561891));
#21281=CARTESIAN_POINT('Ctrl Pts',(4.29423451946808,0.127314547262185,4.54272370785395));
#21282=CARTESIAN_POINT('Ctrl Pts',(4.31809243749951,-0.14829414195428,4.5373703057994));
#21283=CARTESIAN_POINT('Ctrl Pts',(4.34195035553092,-0.387640842632661,
4.40061524972397));
#21284=CARTESIAN_POINT('Ctrl Pts',(4.36580827356235,-0.53219881478122,4.16589884014724));
#21285=CARTESIAN_POINT('Ctrl Pts',(4.38966619159376,-0.546619671109945,
3.89061565172978));
#21286=CARTESIAN_POINT('Ctrl Pts',(4.41352410962518,-0.427377132892538,
3.64207991255526));
#21287=CARTESIAN_POINT('Ctrl Pts',(4.4373820276566,-0.203629241694984,3.48106538615089));
#21288=CARTESIAN_POINT('Ctrl Pts',(4.46123994568802,0.0699115445388116,
3.44694450735191));
#21289=CARTESIAN_POINT('Ctrl Pts',(4.48509786371944,0.326357054473012,3.54806076195131));
#21290=CARTESIAN_POINT('Ctrl Pts',(4.50895578175085,0.502999374434197,3.7596884705576));
#21291=CARTESIAN_POINT('Ctrl Pts',(4.53281369978229,0.556644646112557,4.03007889421215));
#21292=CARTESIAN_POINT('Ctrl Pts',(4.55667161781369,0.474175139017821,4.29311420882242));
#21293=CARTESIAN_POINT('Ctrl Pts',(4.58052953584512,0.275756894216243,4.48447511514554));
#21294=CARTESIAN_POINT('Ctrl Pts',(4.60438745387653,0.00990857728296194,
4.55736865895685));
#21295=CARTESIAN_POINT('Ctrl Pts',(4.62824537190795,-0.258362656684952,
4.49397038324719));
#21296=CARTESIAN_POINT('Ctrl Pts',(4.65210328993938,-0.463457183444019,
4.30978289334447));
#21297=CARTESIAN_POINT('Ctrl Pts',(4.67596120797079,-0.555223804526532,
4.04984504770563));
#21298=CARTESIAN_POINT('Ctrl Pts',(4.69981912600221,-0.511223081411799,
3.77771873014923));
#21299=CARTESIAN_POINT('Ctrl Pts',(4.72367704403363,-0.342214389453536,
3.55994623789246));
#21300=CARTESIAN_POINT('Ctrl Pts',(4.74753496206505,-0.0895249575417115,
3.44977887729433));
#21301=CARTESIAN_POINT('Ctrl Pts',(4.77139288009647,0.185055765100279,3.47415556892044));
#21302=CARTESIAN_POINT('Ctrl Pts',(4.79525079812788,0.414385312357242,3.62711554766008));
#21303=CARTESIAN_POINT('Ctrl Pts',(4.81910871615931,0.542386363113676,3.87125593216545));
#21304=CARTESIAN_POINT('Ctrl Pts',(4.84296663419071,0.537759173780872,4.14687774817434));
#21305=CARTESIAN_POINT('Ctrl Pts',(4.86682455222215,0.401635218192884,4.38658395388507));
#21306=CARTESIAN_POINT('Ctrl Pts',(4.89068247025356,0.167300511433038,4.53175985253543));
#21307=CARTESIAN_POINT('Ctrl Pts',(4.91454038828499,-0.107943727546613,
4.54690598239331));
#21308=CARTESIAN_POINT('Ctrl Pts',(4.9383983063164,-0.356792784813018,4.42831870213619));
#21309=CARTESIAN_POINT('Ctrl Pts',(4.96225622434782,-0.518396287352312,
4.20499583203957));
#21310=CARTESIAN_POINT('Ctrl Pts',(4.98611414237924,-0.553237776802617,
3.93154589703492));
#21311=CARTESIAN_POINT('Ctrl Pts',(5.00997206041066,-0.452797559930213,
3.67483485485756));
#21312=CARTESIAN_POINT('Ctrl Pts',(5.03382997844208,-0.241636005696979,
3.49763554798826));
#21313=CARTESIAN_POINT('Ctrl Pts',(5.05768789647349,0.0286121339618079,
3.44327803376872));
#21314=CARTESIAN_POINT('Ctrl Pts',(5.08154581450492,0.291863827488053,3.52505420509465));
#21315=CARTESIAN_POINT('Ctrl Pts',(5.10540373253633,0.48374686498243,3.72296756053861));
#21316=CARTESIAN_POINT('Ctrl Pts',(5.12926165056775,0.557340616988569,3.98862289364304));
#21317=CARTESIAN_POINT('Ctrl Pts',(5.15311956859917,0.49464940648741,4.25706023915787));
#21318=CARTESIAN_POINT('Ctrl Pts',(5.17697748663059,0.311002942120779,4.46263935401832));
#21319=CARTESIAN_POINT('Ctrl Pts',(5.20083540466201,0.0513077868555636,
4.55509054477827));
#21320=CARTESIAN_POINT('Ctrl Pts',(5.22469332269342,-0.22093351989189,4.5118069769771));
#21321=CARTESIAN_POINT('Ctrl Pts',(5.24855124072485,-0.439150562917527,
4.34337266196288));
#21322=CARTESIAN_POINT('Ctrl Pts',(5.27240915875626,-0.549983331088669,
4.09097437781523));
#21323=CARTESIAN_POINT('Ctrl Pts',(5.29626707678769,-0.526330193563486,
3.81633038019944));
#21324=CARTESIAN_POINT('Ctrl Pts',(5.32012499481911,-0.373974986765411,
3.5865986076849));
#21325=CARTESIAN_POINT('Ctrl Pts',(5.34398291285052,-0.130172708829089,
3.45795473641922));
#21326=CARTESIAN_POINT('Ctrl Pts',(5.36784083088195,0.145460342249349,3.46185569711558));
#21327=CARTESIAN_POINT('Ctrl Pts',(5.39169874891335,0.385524377387638,3.59734759862366));
#21328=CARTESIAN_POINT('Ctrl Pts',(5.41555666694479,0.531317200781484,3.83129898029949));
#21329=CARTESIAN_POINT('Ctrl Pts',(5.4394145849762,0.547188495794237,4.10650235661553));
#21330=CARTESIAN_POINT('Ctrl Pts',(5.46327250300762,0.42925729847004,4.35566300567327));
#21331=CARTESIAN_POINT('Ctrl Pts',(5.48713042103904,0.206360998935678,4.51785436177788));
#21332=CARTESIAN_POINT('Ctrl Pts',(5.51098833907045,-0.0669961859988386,
4.55341622035867));
#21333=CARTESIAN_POINT('Ctrl Pts',(5.53484625710188,-0.323970978517869,
4.45365273830571));
#21334=CARTESIAN_POINT('Ctrl Pts',(5.55870417513329,-0.501726041995696,
4.2429588044862));
#21335=CARTESIAN_POINT('Ctrl Pts',(5.58256209316472,-0.556795421465071,
3.97285482490167));
#21336=CARTESIAN_POINT('Ctrl Pts',(5.60642001119613,-0.475713153578786,
3.70938858005442));
#21337=CARTESIAN_POINT('Ctrl Pts',(5.63027792922756,-0.27830606148521,3.51698474346866));
#21338=CARTESIAN_POINT('Ctrl Pts',(5.65413584725897,-0.0128455564368745,
3.44269129419766));
#21339=CARTESIAN_POINT('Ctrl Pts',(5.67799376529039,0.255756037034639,3.5046750042392));
#21340=CARTESIAN_POINT('Ctrl Pts',(5.70185168332181,0.46181831285622,3.68777916820271));
#21341=CARTESIAN_POINT('Ctrl Pts',(5.72570960135323,0.554953431393631,3.94722983012095));
#21342=CARTESIAN_POINT('Ctrl Pts',(5.74956751938465,0.512387319539865,4.21958423627784));
#21343=CARTESIAN_POINT('Ctrl Pts',(5.77342543741606,0.344528550506956,4.43824431479549));
#21344=CARTESIAN_POINT('Ctrl Pts',(5.79728335544749,0.0924231668635294,
4.54974172178225));
#21345=CARTESIAN_POINT('Ctrl Pts',(5.82114127347891,-0.182282200065281,
4.52681230129395));
#21346=CARTESIAN_POINT('Ctrl Pts',(5.84499919151032,-0.412414601109181,
4.37506292652603));
#21347=CARTESIAN_POINT('Ctrl Pts',(5.86885710954175,-0.541700403334708,
4.13160044316952));
#21348=CARTESIAN_POINT('Ctrl Pts',(5.89271502757316,-0.538525691690445,
3.85595807909033));
#21349=CARTESIAN_POINT('Ctrl Pts',(5.91657294560459,-0.403666797469215,
3.61553786496538));
#21350=CARTESIAN_POINT('Ctrl Pts',(5.94043086363599,-0.170100341263849,
3.46912915944898));
#21351=CARTESIAN_POINT('Ctrl Pts',(5.96428878166742,0.105060216979666,3.45253275189516));
#21352=CARTESIAN_POINT('Ctrl Pts',(5.98814669969884,0.354530812822036,3.5698071562788));
#21353=CARTESIAN_POINT('Ctrl Pts',(6.01200461773026,0.517308736525128,3.79227513259484));
#21354=CARTESIAN_POINT('Ctrl Pts',(6.03586253576167,0.553591019453439,4.06553805729756));
#21355=CARTESIAN_POINT('Ctrl Pts',(6.0597204537931,0.454504394384077,4.32277408438697));
#21356=CARTESIAN_POINT('Ctrl Pts',(6.08357837182452,0.244280620740535,4.50108505220882));
#21357=CARTESIAN_POINT('Ctrl Pts',(6.10743628985593,-0.0256793573627324,
4.55686330558177));
#21358=CARTESIAN_POINT('Ctrl Pts',(6.13129420788736,-0.289354484390735,
4.47648043042773));
#21359=CARTESIAN_POINT('Ctrl Pts',(6.15515212591877,-0.482285035214929,
4.27957167009689));
#21360=CARTESIAN_POINT('Ctrl Pts',(6.17901004395019,-0.557263974895364,
4.01432540012922));
#21361=CARTESIAN_POINT('Ctrl Pts',(6.20286796198161,-0.496014047041978,
3.74552825888183));
#21362=CARTESIAN_POINT('Ctrl Pts',(6.22672588001303,-0.313404643062,3.53904687299508));
#21363=CARTESIAN_POINT('Ctrl Pts',(6.25058379804445,-0.0542924323345977,
3.44511024149985));
#21364=CARTESIAN_POINT('Ctrl Pts',(6.27444171607587,0.218347115212216,3.48718178027374));
#21365=CARTESIAN_POINT('Ctrl Pts',(6.29829963410728,0.437120926894882,3.65404298137615));
#21366=CARTESIAN_POINT('Ctrl Pts',(6.32215755213871,0.549895923261456,3.90664388593688));
#21367=CARTESIAN_POINT('Ctrl Pts',(6.34601547017011,0.526573903738089,4.17995327069166));
#21368=CARTESIAN_POINT('Ctrl Pts',(6.37782602754536,0.327418726170013,4.4906154426808));
#21369=CARTESIAN_POINT('Ctrl Pts',(6.41758922426438,-0.161063729547888,
4.61146011675295));
#21370=CARTESIAN_POINT('Ctrl Pts',(6.46530506032721,-0.60205854017139,4.19446204504257));
#21371=CARTESIAN_POINT('Ctrl Pts',(6.51302089639007,-0.488859252747234,
3.59916283817905));
#21372=CARTESIAN_POINT('Ctrl Pts',(6.56073673245289,0.0725864685289804,
3.37181094029106));
#21373=CARTESIAN_POINT('Ctrl Pts',(6.60845256851574,0.567733426150434,3.72141305678318));
#21374=CARTESIAN_POINT('Ctrl Pts',(6.65616840457857,0.541332409494817,4.32680434473755));
#21375=CARTESIAN_POINT('Ctrl Pts',(6.70388424064141,0.0179179137367747,
4.6321081579338));
#21376=CARTESIAN_POINT('Ctrl Pts',(6.75160007670425,-0.522004047715759,
4.35692568061372));
#21377=CARTESIAN_POINT('Ctrl Pts',(6.79931591276708,-0.582533501572452,
3.75397902491298));
#21378=CARTESIAN_POINT('Ctrl Pts',(6.84703174882993,-0.10812839031349,3.37695395054049));
#21379=CARTESIAN_POINT('Ctrl Pts',(6.89474758489276,0.465580583415614,3.57208337966475));
#21380=CARTESIAN_POINT('Ctrl Pts',(6.9424634209556,0.611735560770294,4.16017430964564));
#21381=CARTESIAN_POINT('Ctrl Pts',(6.99017925701844,0.196126575106773,4.60117519156627));
#21382=CARTESIAN_POINT('Ctrl Pts',(7.03789509308127,-0.399589635450545,
4.49010738789885));
#21383=CARTESIAN_POINT('Ctrl Pts',(7.08561092914412,-0.628355913977057,
3.92896656470948));
#21384=CARTESIAN_POINT('Ctrl Pts',(7.13332676520695,-0.280093617253323,
3.43305676608093));
#21385=CARTESIAN_POINT('Ctrl Pts',(7.1810426012698,0.325383132256395,3.45777970086456));
#21386=CARTESIAN_POINT('Ctrl Pts',(7.22875843733263,0.632055452459012,3.98043185926557));
#21387=CARTESIAN_POINT('Ctrl Pts',(7.27647427339546,0.358301574124045,4.52105375310108));
#21388=CARTESIAN_POINT('Ctrl Pts',(7.32419010945831,-0.244486178793781,
4.58318396235269));
#21389=CARTESIAN_POINT('Ctrl Pts',(7.37190594552114,-0.622758498112341,
4.10976736853928));
#21390=CARTESIAN_POINT('Ctrl Pts',(7.41962178158399,-0.42914211350377,3.53554970961824));
#21391=CARTESIAN_POINT('Ctrl Pts',(7.46733761764681,0.158562080980748,3.38784389968312));
#21392=CARTESIAN_POINT('Ctrl Pts',(7.51505345370967,0.600656274672958,3.80229045545538));
#21393=CARTESIAN_POINT('Ctrl Pts',(7.56276928977248,0.491158570126743,4.3982967283715));
#21394=CARTESIAN_POINT('Ctrl Pts',(7.61048512583535,-0.0693776073840611,
4.62854098691609));
#21395=CARTESIAN_POINT('Ctrl Pts',(7.65820096189817,-0.566203260219877,
4.28158638589565));
#21396=CARTESIAN_POINT('Ctrl Pts',(7.70591679796101,-0.543075747198986,
3.67604667390869));
#21397=CARTESIAN_POINT('Ctrl Pts',(7.75363263402386,-0.0212334191459514,
3.36799828595259));
#21398=CARTESIAN_POINT('Ctrl Pts',(7.80134847008666,0.520107884382028,3.64032679659274));
#21399=CARTESIAN_POINT('Ctrl Pts',(7.84906430614954,0.583826114817312,4.24294874421058));
#21400=CARTESIAN_POINT('Ctrl Pts',(7.89678014221235,0.111407840683781,4.62246712177016));
#21401=CARTESIAN_POINT('Ctrl Pts',(7.94449597827521,-0.463317967772962,
4.43036436352186));
#21402=CARTESIAN_POINT('Ctrl Pts',(7.99221181433803,-0.612571757364041,
3.84305138824375));
#21403=CARTESIAN_POINT('Ctrl Pts',(8.03992765040088,-0.199291476537812,
3.39986673810663));
#21404=CARTESIAN_POINT('Ctrl Pts',(8.08764348646372,0.397001233685627,3.50779369660314));
#21405=CARTESIAN_POINT('Ctrl Pts',(8.13535932252656,0.628721602366905,4.06772127707659));
#21406=CARTESIAN_POINT('Ctrl Pts',(8.18307515858938,0.283077249469033,4.56545936678474));
#21407=CARTESIAN_POINT('Ctrl Pts',(8.23079099465223,-0.32252129731946,4.54392741926377));
#21408=CARTESIAN_POINT('Ctrl Pts',(8.27850683071506,-0.631943574151527,
4.02289855323374));
#21409=CARTESIAN_POINT('Ctrl Pts',(8.32622266677791,-0.361042343138453,
3.48084159342964));
#21410=CARTESIAN_POINT('Ctrl Pts',(8.37393850284074,0.241409626929164,3.41553578665797));
#21411=CARTESIAN_POINT('Ctrl Pts',(8.42165433890358,0.622171422023167,3.88695246013618));
#21412=CARTESIAN_POINT('Ctrl Pts',(8.46937017496642,0.431583626935426,4.46218242893131));
#21413=CARTESIAN_POINT('Ctrl Pts',(8.51708601102927,-0.155334053534803,
4.61298316164806));
#21414=CARTESIAN_POINT('Ctrl Pts',(8.56480184709209,-0.599606082522386,
4.20087202506506));
#21415=CARTESIAN_POINT('Ctrl Pts',(8.61251768315494,-0.493250619804184,
3.60429701705146));
#21416=CARTESIAN_POINT('Ctrl Pts',(8.66023351921777,0.0660644767165412,
3.37110214695249));
#21417=CARTESIAN_POINT('Ctrl Pts',(8.70794935528061,0.564711547735832,3.71543385214437));
#21418=CARTESIAN_POINT('Ctrl Pts',(8.75566519134344,0.544775315265253,4.32108702952508));
#21419=CARTESIAN_POINT('Ctrl Pts',(8.80338102740629,0.0245635283409047,
4.6318810471339));
#21420=CARTESIAN_POINT('Ctrl Pts',(8.85109686346912,-0.518205324617361,
4.36240897642002));
#21421=CARTESIAN_POINT('Ctrl Pts',(8.89881269953197,-0.585098254365674,
3.76013116628075));
#21422=CARTESIAN_POINT('Ctrl Pts',(8.9465285355948,-0.114686454236133,3.3781285970023));
#21423=CARTESIAN_POINT('Ctrl Pts',(8.99424437165764,0.461043681496376,3.56720010581811));
#21424=CARTESIAN_POINT('Ctrl Pts',(9.04196020772047,0.613390310441866,4.15371841694351));
#21425=CARTESIAN_POINT('Ctrl Pts',(9.08967604378332,0.202451179085494,4.59907474052783));
#21426=CARTESIAN_POINT('Ctrl Pts',(9.13739187984615,-0.394401985136886,
4.49429151193569));
#21427=CARTESIAN_POINT('Ctrl Pts',(9.18510771590899,-0.629069737753471,
3.93559278228048));
#21428=CARTESIAN_POINT('Ctrl Pts',(9.23282355197184,-0.28605307070895,3.43604019168954));
#21429=CARTESIAN_POINT('Ctrl Pts',(9.28053938803466,0.319650532659854,3.45438057070715));
#21430=CARTESIAN_POINT('Ctrl Pts',(9.32825522409751,0.631814133431458,3.97377166707843));
#21431=CARTESIAN_POINT('Ctrl Pts',(9.37597106016033,0.363773093762905,4.51724864514637));
#21432=CARTESIAN_POINT('Ctrl Pts',(9.4236868962232,-0.238326375276645,4.58572823348297));
#21433=CARTESIAN_POINT('Ctrl Pts',(9.47140273228601,-0.621567066777005,
4.11632457242483));
#21434=CARTESIAN_POINT('Ctrl Pts',(9.51911856834886,-0.434013156817378,
3.54009826662536));
#21435=CARTESIAN_POINT('Ctrl Pts',(9.5668344044117,0.152101713198456,3.38620679908157));
#21436=CARTESIAN_POINT('Ctrl Pts',(9.61455024047453,0.598539239598464,3.79597107236355));
#21437=CARTESIAN_POINT('Ctrl Pts',(9.66226607653739,0.495328972565208,4.39309824928265));
#21438=CARTESIAN_POINT('Ctrl Pts',(9.7099819126002,-0.0627495115905886,
4.62923725529147));
#21439=CARTESIAN_POINT('Ctrl Pts',(9.75769774866305,-0.563204153727404,
4.28753800770644));
#21440=CARTESIAN_POINT('Ctrl Pts',(9.80541358472588,-0.54645975548653,3.68178818330365));
#21441=CARTESIAN_POINT('Ctrl Pts',(9.85312942078873,-0.027892955418244,
3.36825716649128));
#21442=CARTESIAN_POINT('Ctrl Pts',(9.90084525685157,0.516288374798902,3.63486531430293));
#21443=CARTESIAN_POINT('Ctrl Pts',(9.9485610929144,0.58635414632045,4.2367822623095));
#21444=CARTESIAN_POINT('Ctrl Pts',(9.99627692897723,0.117961883057689,4.62125841547385));
#21445=CARTESIAN_POINT('Ctrl Pts',(10.0439927650401,-0.458756592493822,
4.4352234064191));
#21446=CARTESIAN_POINT('Ctrl Pts',(10.0917086011029,-0.614191830280748,
3.8495160464768));
#21447=CARTESIAN_POINT('Ctrl Pts',(10.1394244371658,-0.205605259764808,
3.40200041654811));
#21448=CARTESIAN_POINT('Ctrl Pts',(10.1871402732286,0.391791784436726,3.5036370055096));
#21449=CARTESIAN_POINT('Ctrl Pts',(10.2348561092915,0.629400404498524,4.06109136983801));
#21450=CARTESIAN_POINT('Ctrl Pts',(10.2825719453542,0.289020948539269,4.56244458923262));
#21451=CARTESIAN_POINT('Ctrl Pts',(10.3302877814171,-0.316770891622519,
4.54729628801251));
#21452=CARTESIAN_POINT('Ctrl Pts',(10.3780036174799,-0.631667147860668,
4.02955738427466));
#21453=CARTESIAN_POINT('Ctrl Pts',(10.4257194535428,-0.366493742769977,
3.48467547975859));
#21454=CARTESIAN_POINT('Ctrl Pts',(10.4734352896056,0.235236505537468,3.41302401146715));
#21455=CARTESIAN_POINT('Ctrl Pts',(10.5211511256685,0.620945451230968,3.88040162523195));
#21456=CARTESIAN_POINT('Ctrl Pts',(10.5688669617313,0.436430634585191,4.45760826680378));
#21457=CARTESIAN_POINT('Ctrl Pts',(10.6165827977941,-0.148865149148659,
4.61458619576145));
#21458=CARTESIAN_POINT('Ctrl Pts',(10.664298633857,-0.597455775834545,4.20718016452724));
#21459=CARTESIAN_POINT('Ctrl Pts',(10.7120144699198,-0.497393570532806,
3.60951740033105));
#21460=CARTESIAN_POINT('Ctrl Pts',(10.7597303059826,0.059432803973042,3.37044081575797));
#21461=CARTESIAN_POINT('Ctrl Pts',(10.8074461420455,0.56168112009921,3.70949811708754));
#21462=CARTESIAN_POINT('Ctrl Pts',(10.8551619781083,0.548129021063343,4.31532776744164));
#21463=CARTESIAN_POINT('Ctrl Pts',(10.9028778141712,0.0312216079359222,
4.63158707701274));
#21464=CARTESIAN_POINT('Ctrl Pts',(10.950593650234,-0.514357088165242,4.36785025554668));
#21465=CARTESIAN_POINT('Ctrl Pts',(10.9983094862968,-0.587593755803164,
3.7663108843084));
#21466=CARTESIAN_POINT('Ctrl Pts',(11.0460253223597,-0.12123403619496,3.37937182377895));
#21467=CARTESIAN_POINT('Ctrl Pts',(11.0937411584225,0.456456764276497,3.56236516706526));
#21468=CARTESIAN_POINT('Ctrl Pts',(11.1414569944854,0.61497629462275,4.14724531131301));
#21469=CARTESIAN_POINT('Ctrl Pts',(11.1891728305482,0.208753630990335,4.59690782052167));
#21470=CARTESIAN_POINT('Ctrl Pts',(11.236888666611,-0.389170704067994,4.49842069353791));
#21471=CARTESIAN_POINT('Ctrl Pts',(11.2846045026739,-0.629713593419695,
3.94222617449013));
#21472=CARTESIAN_POINT('Ctrl Pts',(11.3323203387367,-0.291980800545002,
3.43908624837263));
#21473=CARTESIAN_POINT('Ctrl Pts',(11.3800361747996,0.313882454172263,3.45104205114199));
#21474=CARTESIAN_POINT('Ctrl Pts',(11.4277520108624,0.631502621520784,3.96711438515144));
#21475=CARTESIAN_POINT('Ctrl Pts',(11.4754678469252,0.369204214609944,4.51338608528654));
#21476=CARTESIAN_POINT('Ctrl Pts',(11.5231836829881,-0.232140103514266,
4.58820744384271));
#21477=CARTESIAN_POINT('Ctrl Pts',(11.5708995190509,-0.620306592646703,
4.12286885598323));
#21478=CARTESIAN_POINT('Ctrl Pts',(11.6186153551137,-0.438835993107895,
3.54469790709399));
#21479=CARTESIAN_POINT('Ctrl Pts',(11.6663311911766,0.145624451261577,3.38463787584353));
#21480=CARTESIAN_POINT('Ctrl Pts',(11.7140470272394,0.596355721317347,3.78967435176932));
#21481=CARTESIAN_POINT('Ctrl Pts',(11.7617628633022,0.499444356375145,4.38785610674141));
#21482=CARTESIAN_POINT('Ctrl Pts',(11.8094786993651,-0.0561144459655822,
4.62986363095956));
#21483=CARTESIAN_POINT('Ctrl Pts',(11.8571945354279,-0.560142489144378,
4.29345769116983));
#21484=CARTESIAN_POINT('Ctrl Pts',(11.9049103714908,-0.549783065641843,
3.68756503815187));
#21485=CARTESIAN_POINT('Ctrl Pts',(11.9526262075536,-0.0345493934605723,
3.36858621802886));
#21486=CARTESIAN_POINT('Ctrl Pts',(12.0003420436164,0.512411518346294,3.62944438943981));
#21487=CARTESIAN_POINT('Ctrl Pts',(12.0480578796793,0.588817048391095,4.23058947975914));
#21488=CARTESIAN_POINT('Ctrl Pts',(12.0957737157421,0.1245028227835,4.61998070274044));
#21489=CARTESIAN_POINT('Ctrl Pts',(12.1434895518049,-0.454144260708352,
4.44003410676589));
#21490=CARTESIAN_POINT('Ctrl Pts',(12.1912053878678,-0.615743681684068,
3.85599741975318));
#21491=CARTESIAN_POINT('Ctrl Pts',(12.2389212239306,-0.211896205334937,
3.40420051794564));
#21492=CARTESIAN_POINT('Ctrl Pts',(12.2866370599935,0.386538816815474,3.49953544806202));
#21493=CARTESIAN_POINT('Ctrl Pts',(12.3343528960563,0.63000929582004,4.05445467686));
#21494=CARTESIAN_POINT('Ctrl Pts',(12.3820687321191,0.294932544534008,4.55936733800455));
#21495=CARTESIAN_POINT('Ctrl Pts',(12.429784568182,-0.310985300518122,4.55060436568669));
#21496=CARTESIAN_POINT('Ctrl Pts',(12.4775004042448,-0.631320558980542,
4.0362129322216));
#21497=CARTESIAN_POINT('Ctrl Pts',(12.5252162403077,-0.371904434015698,
3.48856660588983));
#21498=CARTESIAN_POINT('Ctrl Pts',(12.5729320763705,0.229037255191033,3.41057743478371));
#21499=CARTESIAN_POINT('Ctrl Pts',(12.6206479124333,0.619650508764677,3.87386407474765));
#21500=CARTESIAN_POINT('Ctrl Pts',(12.6683637484962,0.44122916559109,4.4529832757215));
#21501=CARTESIAN_POINT('Ctrl Pts',(12.716079584559,-0.142379709528176,4.61612096455669));
#21502=CARTESIAN_POINT('Ctrl Pts',(12.7637954206218,-0.595239106594286,
4.21346529139986));
#21503=CARTESIAN_POINT('Ctrl Pts',(12.8115112566847,-0.501481273143938,
3.61478115656484));
#21504=CARTESIAN_POINT('Ctrl Pts',(12.8592270927475,0.0527945297157079,
3.36984941301012));
#21505=CARTESIAN_POINT('Ctrl Pts',(12.9069429288104,0.558588303589165,3.70359464960132));
#21506=CARTESIAN_POINT('Ctrl Pts',(12.9546587648732,0.551421843290858,4.30953348024615));
#21507=CARTESIAN_POINT('Ctrl Pts',(13.002374600936,0.0378762195828894,4.63122295319618));
#21508=CARTESIAN_POINT('Ctrl Pts',(13.0500904369989,-0.510451719368595,
4.37325067561256));
#21509=CARTESIAN_POINT('Ctrl Pts',(13.0978062730617,-0.590023990114621,
3.77251655941407));
#21510=CARTESIAN_POINT('Ctrl Pts',(13.1455221091246,-0.127768152052348,
3.38068398698829));
#21511=CARTESIAN_POINT('Ctrl Pts',(13.1932379451874,0.451819146005312,3.55757883871291));
#21512=CARTESIAN_POINT('Ctrl Pts',(13.2409537812502,0.616493970155128,4.14075585037205));
#21513=CARTESIAN_POINT('Ctrl Pts',(13.2886696173131,0.215032895532453,4.59467459882739));
#21514=CARTESIAN_POINT('Ctrl Pts',(13.3363854533759,-0.383896195764066,
4.50249451293469));
#21515=CARTESIAN_POINT('Ctrl Pts',(13.3841012894387,-0.630287503488198,
3.94886598394213));
#21516=CARTESIAN_POINT('Ctrl Pts',(13.4318171255016,-0.297876098539286,
3.4421946086935));
#21517=CARTESIAN_POINT('Ctrl Pts',(13.4795329615644,0.308079511111167,3.44776450722078));
#21518=CARTESIAN_POINT('Ctrl Pts',(13.5272487976272,0.631120965295637,3.96046075600252));
#21519=CARTESIAN_POINT('Ctrl Pts',(13.5749646336901,0.374594326004835,4.50946650093658));
#21520=CARTESIAN_POINT('Ctrl Pts',(13.6226804697529,-0.225928046730791,
4.59062131891086));
#21521=CARTESIAN_POINT('Ctrl Pts',(13.6703963058158,-0.618977217803688,
4.12939949185215));
#21522=CARTESIAN_POINT('Ctrl Pts',(13.7181121418786,-0.443610085578744,
3.54934812035851));
#21523=CARTESIAN_POINT('Ctrl Pts',(13.7658279779415,0.139131014051702,3.38313730411011));
#21524=CARTESIAN_POINT('Ctrl Pts',(13.8135438140043,0.594105962672646,3.78340099315002));
#21525=CARTESIAN_POINT('Ctrl Pts',(13.8612596500671,0.503504264276035,4.38257088298437));
#21526=CARTESIAN_POINT('Ctrl Pts',(13.90897548613,-0.0494731474142026,4.63042004436449));
#21527=CARTESIAN_POINT('Ctrl Pts',(13.9566913221928,-0.557018606591754,
4.29934477874546));
#21528=CARTESIAN_POINT('Ctrl Pts',(14.0044071582556,-0.553045308503159,
3.69337659679301));
#21529=CARTESIAN_POINT('Ctrl Pts',(14.0521229943185,-0.0412019939202257,
3.36898540401303));
#21530=CARTESIAN_POINT('Ctrl Pts',(14.0998388303813,0.50847774565382,3.62406462413548));
#21531=CARTESIAN_POINT('Ctrl Pts',(14.1475546664442,0.591214547458171,4.22437108442359));
#21532=CARTESIAN_POINT('Ctrl Pts',(14.195270502507,0.131029933326566,4.61863412549262));
#21533=CARTESIAN_POINT('Ctrl Pts',(14.2429863385698,-0.4494814847335,4.44479593021223));
#21534=CARTESIAN_POINT('Ctrl Pts',(14.2907021746327,-0.617227139201166,
3.86249478815283));
#21535=CARTESIAN_POINT('Ctrl Pts',(14.3384180106955,-0.218163614480107,
3.40646679792233));
#21536=CARTESIAN_POINT('Ctrl Pts',(14.3861338467583,0.381242914296727,3.49548947984197));
#21537=CARTESIAN_POINT('Ctrl Pts',(14.4338496828212,0.630548208698617,4.0478119353149));
#21538=CARTESIAN_POINT('Ctrl Pts',(14.481565518884,0.300811380821271,4.55622795490698));
#21539=CARTESIAN_POINT('Ctrl Pts',(14.5292813549469,-0.305165166642291,
4.55385128484077));
#21540=CARTESIAN_POINT('Ctrl Pts',(14.5769971910097,-0.630903846008588,
4.04286445780787));
#21541=CARTESIAN_POINT('Ctrl Pts',(14.6247130270726,-0.37727381588172,3.49251453961553));
#21542=CARTESIAN_POINT('Ctrl Pts',(14.6724288631354,0.222812564473163,3.40819632836178));
#21543=CARTESIAN_POINT('Ctrl Pts',(14.7201446991982,0.618286738460357,3.86734053484336));
#21544=CARTESIAN_POINT('Ctrl Pts',(14.7678605352611,0.44597868695508,4.44830796940654));
#21545=CARTESIAN_POINT('Ctrl Pts',(14.8155763713239,-0.135878455045208,
4.6175872975589));
#21546=CARTESIAN_POINT('Ctrl Pts',(14.8632922073867,-0.592956321018707,
4.2197267075609));
#21547=CARTESIAN_POINT('Ctrl Pts',(14.9110080434496,-0.505513273594975,
3.62008770107973));
#21548=CARTESIAN_POINT('Ctrl Pts',(14.9587238795124,0.0461503912925444,
3.36932800439917));
#21549=CARTESIAN_POINT('Ctrl Pts',(15.0064397155752,0.555433441741075,3.69772410541485));
#21550=CARTESIAN_POINT('Ctrl Pts',(15.0541555516381,0.554653416196733,4.30370481154056));
#21551=CARTESIAN_POINT('Ctrl Pts',(15.1018713877009,0.0445266241191229,
4.63078871612938));
#21552=CARTESIAN_POINT('Ctrl Pts',(15.1495872237638,-0.506489652017253,
4.37860963676461));
#21553=CARTESIAN_POINT('Ctrl Pts',(15.1973030598266,-0.592388687361149,
3.77874750230084));
#21554=CARTESIAN_POINT('Ctrl Pts',(15.2450188958894,-0.134288076029725,
3.38206494088146));
#21555=CARTESIAN_POINT('Ctrl Pts',(15.2927347319523,0.447131341807447,3.5528416524037));
#21556=CARTESIAN_POINT('Ctrl Pts',(15.3404505680151,0.617943168462805,4.13425075493917));
#21557=CARTESIAN_POINT('Ctrl Pts',(15.3881664040779,0.221288275240951,4.59237532350063));
#21558=CARTESIAN_POINT('Ctrl Pts',(15.4358822401408,-0.378579046092452,
4.50651251762549));
#21559=CARTESIAN_POINT('Ctrl Pts',(15.4835980762036,-0.630791404211772,
3.95551147311801));
#21560=CARTESIAN_POINT('Ctrl Pts',(15.5313139122665,-0.303738309870084,
3.44536492739022));
#21561=CARTESIAN_POINT('Ctrl Pts',(15.5790297483293,0.302242348039936,3.44454830299756));
#21562=CARTESIAN_POINT('Ctrl Pts',(15.6267455843921,0.630669207148581,3.95381151868517));
#21563=CARTESIAN_POINT('Ctrl Pts',(15.674461420455,0.379942829239589,4.50549032746533));
#21564=CARTESIAN_POINT('Ctrl Pts',(15.7221772565178,-0.219690894932002,
4.59296959056563));
#21565=CARTESIAN_POINT('Ctrl Pts',(15.7698930925806,-0.617579089908608,
4.13591575463957));
#21566=CARTESIAN_POINT('Ctrl Pts',(15.8176089286435,-0.448334903946386,
3.5540483898953));
#21567=CARTESIAN_POINT('Ctrl Pts',(15.8653247647063,0.13262212282903,3.3817052505577));
#21568=CARTESIAN_POINT('Ctrl Pts',(15.9130406007692,0.591790213556878,3.77715169332057));
#21569=CARTESIAN_POINT('Ctrl Pts',(15.960756436832,0.507508245312566,4.37724316506909));
#21570=CARTESIAN_POINT('Ctrl Pts',(16.0084722728949,-0.0428263536203826,
4.63090643370248));
#21571=CARTESIAN_POINT('Ctrl Pts',(16.0561881089577,-0.553832853055588,
4.30519861652357));
#21572=CARTESIAN_POINT('Ctrl Pts',(16.1039039450205,-0.556246121716014,
3.69922221370673));
#21573=CARTESIAN_POINT('Ctrl Pts',(16.1516197810833,-0.0478500178579074,
3.36945468010413));
#21574=CARTESIAN_POINT('Ctrl Pts',(16.1993356171462,0.504487493666278,3.61872661594874));
#21575=CARTESIAN_POINT('Ctrl Pts',(16.247051453209,0.593546377218863,4.21812776701271));
#21576=CARTESIAN_POINT('Ctrl Pts',(16.2947672892719,0.137542489686435,4.61721883330181));
#21577=CARTESIAN_POINT('Ctrl Pts',(16.3424831253347,-0.444768782488292,
4.44950834783736));
#21578=CARTESIAN_POINT('Ctrl Pts',(16.3901989613976,-0.618642038056621,
3.86900742997889));
#21579=CARTESIAN_POINT('Ctrl Pts',(16.4379147974604,-0.224406791046256,
3.40879900475058));
#21580=CARTESIAN_POINT('Ctrl Pts',(16.4856306335233,0.375904665124208,3.49149955025639));
#21581=CARTESIAN_POINT('Ctrl Pts',(16.533346469586,0.631017083274371,4.04116388304691));
#21582=CARTESIAN_POINT('Ctrl Pts',(16.5810623056489,0.306656804407812,4.55302678864769));
#21583=CARTESIAN_POINT('Ctrl Pts',(16.6287781417117,-0.29931113646787,4.55703668482238));
#21584=CARTESIAN_POINT('Ctrl Pts',(16.6764939777746,-0.630417055231307,
4.04951122221356));
#21585=CARTESIAN_POINT('Ctrl Pts',(16.7242098138374,-0.382601291962586,
3.49651884241796));
#21586=CARTESIAN_POINT('Ctrl Pts',(16.7719256499003,0.216563124792967,3.40588095668335));
#21587=CARTESIAN_POINT('Ctrl Pts',(16.8196414859631,0.616854291799135,3.86083173012294));
#21588=CARTESIAN_POINT('Ctrl Pts',(16.8673573220259,0.450678671122871,4.44358286716973));
#21589=CARTESIAN_POINT('Ctrl Pts',(16.9150731580887,-0.129362107828251,
4.61898503189482));
#21590=CARTESIAN_POINT('Ctrl Pts',(16.9627889941516,-0.590607672668797,
4.22596371752193));
#21591=CARTESIAN_POINT('Ctrl Pts',(17.0105048302144,-0.509489124030439,
3.62543644444997));
#21592=CARTESIAN_POINT('Ctrl Pts',(17.0582206662773,0.0395011267029154,
3.3688766478407));
#21593=CARTESIAN_POINT('Ctrl Pts',(17.1059365023401,0.552216884982031,3.69188713660034));
#21594=CARTESIAN_POINT('Ctrl Pts',(17.153652338403,0.557823380833178,4.29784240874569));
#21595=CARTESIAN_POINT('Ctrl Pts',(17.2013681744658,0.0511720828492506,
4.63028441404532));
#21596=CARTESIAN_POINT('Ctrl Pts',(17.2490840105287,-0.502471326198846,
4.38392654375487));
#21597=CARTESIAN_POINT('Ctrl Pts',(17.2967998465914,-0.594687584883411,
3.78500302086511));
#21598=CARTESIAN_POINT('Ctrl Pts',(17.3445156826543,-0.140793083924855,
3.38351453206865));
#21599=CARTESIAN_POINT('Ctrl Pts',(17.3922315187171,0.442393872381948,3.5481541343218));
#21600=CARTESIAN_POINT('Ctrl Pts',(17.43994735478,0.61932372857571,4.1277307475695));
#21601=CARTESIAN_POINT('Ctrl Pts',(17.4876631908428,0.227519075297936,4.590010249934));
#21602=CARTESIAN_POINT('Ctrl Pts',(17.5353790269057,-0.373219845656906,
4.51047426130944));
#21603=CARTESIAN_POINT('Ctrl Pts',(17.5830948629685,-0.631225239619516,
3.96216190386831));
#21604=CARTESIAN_POINT('Ctrl Pts',(17.6308106990313,-0.309566783390781,
3.44859685231885));
#21605=CARTESIAN_POINT('Ctrl Pts',(17.6785265350942,0.29637161332294,3.44139379571298));
#21606=CARTESIAN_POINT('Ctrl Pts',(17.726242371157,0.630147397258769,3.94716741176515));
#21607=CARTESIAN_POINT('Ctrl Pts',(17.7739582072198,0.385249130227842,4.50145800652724));
#21608=CARTESIAN_POINT('Ctrl Pts',(17.8216740432827,-0.213429340911116,
4.59525199797214));
#21609=CARTESIAN_POINT('Ctrl Pts',(17.8693898793456,-0.616112364258878,
4.14241692054995));
#21610=CARTESIAN_POINT('Ctrl Pts',(17.9171057154084,-0.453009923400427,
3.55879819362073));
#21611=CARTESIAN_POINT('Ctrl Pts',(17.9648215514712,0.126098500570276,3.38034187425201));
#21612=CARTESIAN_POINT('Ctrl Pts',(18.012537387534,0.589408731192455,3.77092714642348));
#21613=CARTESIAN_POINT('Ctrl Pts',(18.0602532235969,0.511455854741549,4.3718735447732));
#21614=CARTESIAN_POINT('Ctrl Pts',(18.1079690596597,-0.0361748028784226,
4.6313227449477));
#21615=CARTESIAN_POINT('Ctrl Pts',(18.1556848957226,-0.55058558239424,4.31101855428765));
#21616=CARTESIAN_POINT('Ctrl Pts',(18.2034007317854,-0.559385149749292,
3.70510123958967));
#21617=CARTESIAN_POINT('Ctrl Pts',(18.2511165678482,-0.0544927268426965,
3.36999399417717));
#21618=CARTESIAN_POINT('Ctrl Pts',(18.2988324039111,0.500441205601937,3.6134309578002));
#21619=CARTESIAN_POINT('Ctrl Pts',(18.3465482399739,0.595812278664582,4.21186022100458));
#21620=CARTESIAN_POINT('Ctrl Pts',(18.3942640760367,0.144039768479226,4.61573498337195));
#21621=CARTESIAN_POINT('Ctrl Pts',(18.4419799120996,-0.440006677437314,
4.4541708362083));
#21622=CARTESIAN_POINT('Ctrl Pts',(18.4896957481624,-0.619988221090196,
3.87553462183804));
#21623=CARTESIAN_POINT('Ctrl Pts',(18.5374115842252,-0.230625041570952,
3.41119687937986));
#21624=CARTESIAN_POINT('Ctrl Pts',(18.5851274202881,0.370524662245315,3.48756610248778));
#21625=CARTESIAN_POINT('Ctrl Pts',(18.6328432563509,0.631415867466904,4.03451125849008));
#21626=CARTESIAN_POINT('Ctrl Pts',(18.6805590924138,0.31246816601179,4.54976419479712));
#21627=CARTESIAN_POINT('Ctrl Pts',(18.7282749284766,-0.293423860232864,
4.56016021181225));
#21628=CARTESIAN_POINT('Ctrl Pts',(18.7759907645394,-0.629860240718928,
4.05615248714788));
#21629=CARTESIAN_POINT('Ctrl Pts',(18.8237066006023,-0.387886270507855,
3.50057906951772));
#21630=CARTESIAN_POINT('Ctrl Pts',(18.8714224366651,0.210289630309142,3.40363157692976));
#21631=CARTESIAN_POINT('Ctrl Pts',(18.919138272728,0.615353327889266,3.85433838355196));
#21632=CARTESIAN_POINT('Ctrl Pts',(18.9668541087908,0.455328596044662,4.43880849385601));
#21633=CARTESIAN_POINT('Ctrl Pts',(19.0145699448537,-0.122831391686292,
4.62031401230505));
#21634=CARTESIAN_POINT('Ctrl Pts',(19.0622857809165,-0.588193422413584,
4.2321756285162));
#21635=CARTESIAN_POINT('Ctrl Pts',(19.1100016169793,-0.513408382846255,
3.63082679254236));
#21636=CARTESIAN_POINT('Ctrl Pts',(19.1577174530421,0.0328474745430158,
3.36849539350727));
#21637=CARTESIAN_POINT('Ctrl Pts',(19.205433289105,0.548938990540088,3.68608439142882));
#21638=CARTESIAN_POINT('Ctrl Pts',(19.2531491251678,0.560931385193363,4.2919469231649));
#21639=CARTESIAN_POINT('Ctrl Pts',(19.3008649612307,0.0578118574426247,
4.62971010270368));
#21640=CARTESIAN_POINT('Ctrl Pts',(19.3485807972935,-0.498397187901359,
4.38920080648958));
#21641=CARTESIAN_POINT('Ctrl Pts',(19.3962966333563,-0.596920427988996,
3.79128241936144));
#21642=CARTESIAN_POINT('Ctrl Pts',(19.4440124694192,-0.147282451949449,
3.38503260125846));
#21643=CARTESIAN_POINT('Ctrl Pts',(19.491728305482,0.437607261597584,3.54351680188243));
#21644=CARTESIAN_POINT('Ctrl Pts',(19.5394441415449,0.620635501579114,4.12119655861503));
#21645=CARTESIAN_POINT('Ctrl Pts',(19.5871599776077,0.233724595248439,4.58757962923414));
#21646=CARTESIAN_POINT('Ctrl Pts',(19.6348758136705,-0.367819173932889,
4.51437932582758));
#21647=CARTESIAN_POINT('Ctrl Pts',(19.6825916497334,-0.631588991354928,
3.96881649615688));
#21648=CARTESIAN_POINT('Ctrl Pts',(19.7303074857962,-0.315360815373557,
3.4518901025469));
#21649=CARTESIAN_POINT('Ctrl Pts',(19.778023321859,0.290467852693633,3.43830118837221));
#21650=CARTESIAN_POINT('Ctrl Pts',(19.8257391579219,0.629555794415491,3.94052945152661));
#21651=CARTESIAN_POINT('Ctrl Pts',(19.8734549939847,0.390512260364629,4.49736946054851));
#21652=CARTESIAN_POINT('Ctrl Pts',(19.9211708300476,-0.207143364153331,
4.59746927979605));
#21653=CARTESIAN_POINT('Ctrl Pts',(19.9688866661104,-0.61457855576007,4.14890039401813));
#21654=CARTESIAN_POINT('Ctrl Pts',(20.0166025021732,-0.45763207183192,3.5636005413983));
#21655=CARTESIAN_POINT('Ctrl Pts',(20.0643183382361,0.119556051622903,3.37904064719698));
#21656=CARTESIAN_POINT('Ctrl Pts',(20.1120341742989,0.586970881772813,3.7647406560623));
#21657=CARTESIAN_POINT('Ctrl Pts',(20.1597500103618,0.515329468049299,4.36643880344312));
#21658=CARTESIAN_POINT('Ctrl Pts',(20.2074658464246,-0.029486781418557,
4.63171390504007));
#21659=CARTESIAN_POINT('Ctrl Pts',(20.2551816824874,-0.547338447674763,
4.31671898245684));
#21660=CARTESIAN_POINT('Ctrl Pts',(20.3028975185503,-0.562346186529673,
3.71117381387971));
#21661=CARTESIAN_POINT('Ctrl Pts',(20.3506133546131,-0.0613491664957494,
3.37029669484294));
#21662=CARTESIAN_POINT('Ctrl Pts',(20.398329190676,0.496762641213801,3.60878154740643));
#21663=CARTESIAN_POINT('Ctrl Pts',(20.4380923873949,0.580417208789547,4.10498761157686));
#21664=CARTESIAN_POINT('Ctrl Pts',(20.4699029447702,0.374745574175769,4.41137453781958));
#21665=CARTESIAN_POINT('Ctrl Pts',(20.4937608628016,0.13332385162888,4.54159545884303));
#21666=CARTESIAN_POINT('Ctrl Pts',(20.517618780833,-0.143293564288956,4.53872805560682));
#21667=CARTESIAN_POINT('Ctrl Pts',(20.5414766988645,-0.38346854803195,4.40448715909776));
#21668=CARTESIAN_POINT('Ctrl Pts',(20.5653346168959,-0.530621786340447,
4.17114564603877));
#21669=CARTESIAN_POINT('Ctrl Pts',(20.5891925349273,-0.547627617499454,
3.89605651468078));
#21670=CARTESIAN_POINT('Ctrl Pts',(20.6130504529587,-0.430933317123153,
3.64633026976583));
#21671=CARTESIAN_POINT('Ctrl Pts',(20.6369083709901,-0.208752997660079,
3.48311457674551));
#21672=CARTESIAN_POINT('Ctrl Pts',(20.6607662890215,0.0644142843662171,
3.4462762657402));
#21673=CARTESIAN_POINT('Ctrl Pts',(20.684624207053,0.321861676845817,3.54484653226013));
#21674=CARTESIAN_POINT('Ctrl Pts',(20.7084821250844,0.500588620804837,3.75470996102831));
#21675=CARTESIAN_POINT('Ctrl Pts',(20.7323400431158,0.556916750317041,4.02455574134091));
#21676=CARTESIAN_POINT('Ctrl Pts',(20.7561979611472,0.47705893600668,4.28839577951569));
#21677=CARTESIAN_POINT('Ctrl Pts',(20.7800558791787,0.280549668164313,4.48171582646486));
#21678=CARTESIAN_POINT('Ctrl Pts',(20.8039137972101,0.0154370662995263,
4.55724289713534));
#21679=CARTESIAN_POINT('Ctrl Pts',(20.8277717152415,-0.253449631274377,
4.49650907789895));
#21680=CARTESIAN_POINT('Ctrl Pts',(20.8516296332729,-0.460361354274216,
4.31436517051053));
#21681=CARTESIAN_POINT('Ctrl Pts',(20.8754875513043,-0.554701993332711,
4.05535046556385));
#21682=CARTESIAN_POINT('Ctrl Pts',(20.8993454693358,-0.513402987365846,
3.78280103771366));
#21683=CARTESIAN_POINT('Ctrl Pts',(20.9232033873672,-0.346562912086465,
3.56336268648205));
#21684=CARTESIAN_POINT('Ctrl Pts',(20.9470613053986,-0.0949787932613798,
3.45069404477467));
#21685=CARTESIAN_POINT('Ctrl Pts',(20.97091922343,0.179830242856268,3.47234567582879));
#21686=CARTESIAN_POINT('Ctrl Pts',(20.9947771414614,0.410665878084123,3.62302316008453));
#21687=CARTESIAN_POINT('Ctrl Pts',(21.0186350594928,0.541082524061315,3.86588175144064));
#21688=CARTESIAN_POINT('Ctrl Pts',(21.0424929775243,0.539189751860116,4.14153590729571));
#21689=CARTESIAN_POINT('Ctrl Pts',(21.0663508955557,0.405450399288564,4.38258067876424));
#21690=CARTESIAN_POINT('Ctrl Pts',(21.0902088135871,0.172567379211795,4.53007405282339));
#21691=CARTESIAN_POINT('Ctrl Pts',(21.1140667316185,-0.102513065388571,
4.54794988212627));
#21692=CARTESIAN_POINT('Ctrl Pts',(21.1379246496499,-0.352526273278862,
4.43183703934844));
#21693=CARTESIAN_POINT('Ctrl Pts',(21.1617825676814,-0.516337204635697,
4.21012827746935));
#21694=CARTESIAN_POINT('Ctrl Pts',(21.1856404857128,-0.553889624765765,
3.93703742795684));
#21695=CARTESIAN_POINT('Ctrl Pts',(21.2094984037442,-0.456000943963824,
3.67934264238169));
#21696=CARTESIAN_POINT('Ctrl Pts',(21.2333563217756,-0.246607611160355,
3.50005731527167));
#21697=CARTESIAN_POINT('Ctrl Pts',(21.257214239807,0.0230880000356606,3.44302159274494));
#21698=CARTESIAN_POINT('Ctrl Pts',(21.2810721578385,0.287137966314551,3.52218226257825));
#21699=CARTESIAN_POINT('Ctrl Pts',(21.3049300758698,0.480974878350452,3.71818238470557));
#21700=CARTESIAN_POINT('Ctrl Pts',(21.3287879939013,0.557200331135927,3.9830945903298));
#21701=CARTESIAN_POINT('Ctrl Pts',(21.3526459119327,0.497175125126959,4.25214062911267));
#21702=CARTESIAN_POINT('Ctrl Pts',(21.3765038299641,0.31557705824565,4.45953141590455));
#21703=CARTESIAN_POINT('Ctrl Pts',(21.4003617479955,0.0568118044769688,
4.55455425412338));
#21704=CARTESIAN_POINT('Ctrl Pts',(21.424219666027,-0.215845483008899,4.51397347145443));
#21705=CARTESIAN_POINT('Ctrl Pts',(21.4480775840584,-0.435722670386138,
4.34771217465862));
#21706=CARTESIAN_POINT('Ctrl Pts',(21.4719355020898,-0.549053796006754,
4.0964257796693));
#21707=CARTESIAN_POINT('Ctrl Pts',(21.4957934201212,-0.528126312578589,
3.82156065496534));
#21708=CARTESIAN_POINT('Ctrl Pts',(21.5196513381527,-0.378057559853047,
3.59032881071252));
#21709=CARTESIAN_POINT('Ctrl Pts',(21.543509256184,-0.135543435662257,3.45927273145963));
#21710=CARTESIAN_POINT('Ctrl Pts',(21.5673671742155,0.14011475067701,3.46043919847993));
#21711=CARTESIAN_POINT('Ctrl Pts',(21.5912250922469,0.381511063826562,3.59354297881304));
#21712=CARTESIAN_POINT('Ctrl Pts',(21.6150830102783,0.529617529717794,3.8260365724933));
#21713=CARTESIAN_POINT('Ctrl Pts',(21.6389409283097,0.548218083101175,4.10106896286759));
#21714=CARTESIAN_POINT('Ctrl Pts',(21.6627988463412,0.432764382005563,4.35138723875747));
#21715=CARTESIAN_POINT('Ctrl Pts',(21.6866567643726,0.211488001244504,4.51578176317496));
#21716=CARTESIAN_POINT('Ctrl Pts',(21.710514682404,-0.0615029566383307,
4.55405359688301));
#21717=CARTESIAN_POINT('Ctrl Pts',(21.7343726004354,-0.319454766316188,
4.4568442340362));
#21718=CARTESIAN_POINT('Ctrl Pts',(21.7582305184669,-0.499291183856609,
4.24792401178047));
#21719=CARTESIAN_POINT('Ctrl Pts',(21.7820884364982,-0.557037306525311,
3.97837961532992));
#21720=CARTESIAN_POINT('Ctrl Pts',(21.8059463545297,-0.478572634356998,
3.71412199185867));
#21721=CARTESIAN_POINT('Ctrl Pts',(21.8298042725611,-0.283083917031579,
3.51976932853855));
#21722=CARTESIAN_POINT('Ctrl Pts',(21.8536621905926,-0.018373470940863,
3.44284614561161));
#21723=CARTESIAN_POINT('Ctrl Pts',(21.8775201086239,0.250829789278194,3.5021622566489));
#21724=CARTESIAN_POINT('Ctrl Pts',(21.9013780266554,0.458698333552465,3.68321325676341));
#21725=CARTESIAN_POINT('Ctrl Pts',(21.9252359446868,0.55440264058141,3.94172724469688));
#21726=CARTESIAN_POINT('Ctrl Pts',(21.9490938627182,0.514540400363477,4.21449050861997));
#21727=CARTESIAN_POINT('Ctrl Pts',(21.9729517807496,0.348859016457567,4.4348050005813));
#21728=CARTESIAN_POINT('Ctrl Pts',(21.996809698781,0.0978721002989983,4.54879782605011));
#21729=CARTESIAN_POINT('Ctrl Pts',(22.0206676168125,-0.177047210365213,
4.52859463409701));
#21730=CARTESIAN_POINT('Ctrl Pts',(22.0445255348439,-0.408673655425848,
4.3791356554785));
#21731=CARTESIAN_POINT('Ctrl Pts',(22.0683834528753,-0.540368259688198,
4.13696768164748));
#21732=CARTESIAN_POINT('Ctrl Pts',(22.0922413709067,-0.53992810512055,3.86130737872913));
#21733=CARTESIAN_POINT('Ctrl Pts',(22.1160992889381,-0.407460821505317,
3.61956119962225));
#21734=CARTESIAN_POINT('Ctrl Pts',(22.1399572069695,-0.175358268020808,
3.47084267015335));
#21735=CARTESIAN_POINT('Ctrl Pts',(22.163815125001,0.0996241586556461,3.45151752178681));
#21736=CARTESIAN_POINT('Ctrl Pts',(22.1876730430324,0.350245764837839,3.56631127970877));
#21737=CARTESIAN_POINT('Ctrl Pts',(22.2115309610638,0.51522274100534,3.78715374318048));
#21738=CARTESIAN_POINT('Ctrl Pts',(22.2353888790952,0.554213722627899,4.06004291426965));
#21739=CARTESIAN_POINT('Ctrl Pts',(22.2592467971266,0.457684352558003,4.31824995726588));
#21740=CARTESIAN_POINT('Ctrl Pts',(22.2831047151581,0.249238691275201,4.49863621678958));
#21741=CARTESIAN_POINT('Ctrl Pts',(22.3069626331895,-0.0201526192614011,
4.55709233866662));
#21742=CARTESIAN_POINT('Ctrl Pts',(22.3308205512209,-0.284616065231974,
4.47932420896945));
#21743=CARTESIAN_POINT('Ctrl Pts',(22.3546784692523,-0.479483130864429,
4.28434825342259));
#21744=CARTESIAN_POINT('Ctrl Pts',(22.3785363872838,-0.557103509392546,
4.01984140485232));
#21745=CARTESIAN_POINT('Ctrl Pts',(22.4023943053151,-0.498496906094933,
3.75048279151596));
#21746=CARTESIAN_POINT('Ctrl Pts',(22.4262522233466,-0.317994227800984,
3.542137933897));
#21747=CARTESIAN_POINT('Ctrl Pts',(22.450110141378,-0.0597333038680864,
3.44575282046209));
#21748=CARTESIAN_POINT('Ctrl Pts',(22.4739680594094,0.213134049493302,3.48489624527193));
#21749=CARTESIAN_POINT('Ctrl Pts',(22.4978259774408,0.433884304103661,3.6499965589521));
#21750=CARTESIAN_POINT('Ctrl Pts',(22.5216838954723,0.548538061567711,3.90068226732924));
#21751=CARTESIAN_POINT('Ctrl Pts',(22.5455418135037,0.529059256943919,4.17565382996358));
#21752=CARTESIAN_POINT('Ctrl Pts',(22.5693997315351,0.380211173855379,4.40767331583304));
#21753=CARTESIAN_POINT('Ctrl Pts',(22.5932576495665,0.138390873272415,4.54000544018811));
#21754=CARTESIAN_POINT('Ctrl Pts',(22.6171155675979,-0.137269333605106,
4.54029177230974));
#21755=CARTESIAN_POINT('Ctrl Pts',(22.6409734856293,-0.379364264814148,
4.40846158181013));
#21756=CARTESIAN_POINT('Ctrl Pts',(22.6648314036608,-0.528692759685234,
4.17675229015827));
#21757=CARTESIAN_POINT('Ctrl Pts',(22.6886893216921,-0.54874438127821,3.90182058373076));
#21758=CARTESIAN_POINT('Ctrl Pts',(22.7125472397236,-0.434607562942265,
3.65089956353622));
#21759=CARTESIAN_POINT('Ctrl Pts',(22.736405157755,-0.214207731687487,3.48533716867003));
#21760=CARTESIAN_POINT('Ctrl Pts',(22.7602630757864,0.0585913648593265,
3.44563509732658));
#21761=CARTESIAN_POINT('Ctrl Pts',(22.7841209938179,0.31702578011682,3.5414689143437));
#21762=CARTESIAN_POINT('Ctrl Pts',(22.8079789118493,0.498012898707086,3.74946820019106));
#21763=CARTESIAN_POINT('Ctrl Pts',(22.8238841905369,0.537376264140017,3.92891364167179));
#21764=CARTESIAN_POINT('Ctrl Pts',(22.8318368298807,0.534391234777113,4.01792167950194));
#21765=CARTESIAN_POINT('Ctrl Pts',(3.99999999999998,0.254694598474614,4.53673594206822));
#21766=CARTESIAN_POINT('Ctrl Pts',(4.00795263934379,0.165296026927429,4.57915779516171));
#21767=CARTESIAN_POINT('Ctrl Pts',(4.0238579180314,-0.0350146299391769,
4.61842892627033));
#21768=CARTESIAN_POINT('Ctrl Pts',(4.04771583606282,-0.327086058023631,
4.5259865276721));
#21769=CARTESIAN_POINT('Ctrl Pts',(4.07157375409423,-0.539100294705402,
4.30498302442502));
#21770=CARTESIAN_POINT('Ctrl Pts',(4.09543167212566,-0.619328256935644,
4.00937412827253));
#21771=CARTESIAN_POINT('Ctrl Pts',(4.11928959015708,-0.548093442686671,
3.71148804617917));
#21772=CARTESIAN_POINT('Ctrl Pts',(4.1431475081885,-0.342845496867427,3.48414304986991));
#21773=CARTESIAN_POINT('Ctrl Pts',(4.16700542621991,-0.0537568536316998,
3.38294333505492));
#21774=CARTESIAN_POINT('Ctrl Pts',(4.19086334425134,0.248473820944083,3.43262855616194));
#21775=CARTESIAN_POINT('Ctrl Pts',(4.21472126228276,0.489947458130694,3.62105272953394));
#21776=CARTESIAN_POINT('Ctrl Pts',(4.23857918031417,0.611614759069978,3.90213920826301));
#21777=CARTESIAN_POINT('Ctrl Pts',(4.26243709834559,0.583726034554802,4.20715564703007));
#21778=CARTESIAN_POINT('Ctrl Pts',(4.28629501637702,0.413100159498109,4.46151671210738));
#21779=CARTESIAN_POINT('Ctrl Pts',(4.31015293440843,0.141460167127662,4.60302446238992));
#21780=CARTESIAN_POINT('Ctrl Pts',(4.33401085243986,-0.164770755236008,
4.59707625642582));
#21781=CARTESIAN_POINT('Ctrl Pts',(4.35786877047126,-0.430710704813839,
4.44512666775742));
#21782=CARTESIAN_POINT('Ctrl Pts',(4.38172668850269,-0.59133017320549,4.18433147003372));
#21783=CARTESIAN_POINT('Ctrl Pts',(4.40558460653411,-0.607353296958831,
3.87846221409715));
#21784=CARTESIAN_POINT('Ctrl Pts',(4.42944252456553,-0.474862000813124,
3.60231225357117));
#21785=CARTESIAN_POINT('Ctrl Pts',(4.45330044259694,-0.226254007744579,
3.42340778189093));
#21786=CARTESIAN_POINT('Ctrl Pts',(4.47715836062837,0.0776792518003291,
3.38549581251083));
#21787=CARTESIAN_POINT('Ctrl Pts',(4.50101627865978,0.362617819109035,3.49784685630402));
#21788=CARTESIAN_POINT('Ctrl Pts',(4.5248741966912,0.558886451727075,3.73298802180378));
#21789=CARTESIAN_POINT('Ctrl Pts',(4.54873211472262,0.618492123352341,4.03342088939383));
#21790=CARTESIAN_POINT('Ctrl Pts',(4.57259003275404,0.5268596233165,4.32568143907503));
#21791=CARTESIAN_POINT('Ctrl Pts',(4.59644795078546,0.306395594072305,4.5383040055633));
#21792=CARTESIAN_POINT('Ctrl Pts',(4.62030586881688,0.0110094959969652,
4.61929657956068));
#21793=CARTESIAN_POINT('Ctrl Pts',(4.6441637868483,-0.287068723725306,4.54885427056805));
#21794=CARTESIAN_POINT('Ctrl Pts',(4.66802170487971,-0.514950820910697,
4.34420214192463));
#21795=CARTESIAN_POINT('Ctrl Pts',(4.69187962291114,-0.616913415399932,
4.05538321370614));
#21796=CARTESIAN_POINT('Ctrl Pts',(4.71573754094255,-0.568023875442366,
3.75302158112612));
#21797=CARTESIAN_POINT('Ctrl Pts',(4.73959545897398,-0.380237025278099,
3.51105289951885));
#21798=CARTESIAN_POINT('Ctrl Pts',(4.76345337700539,-0.0994718649854296,
3.38864510263028));
#21799=CARTESIAN_POINT('Ctrl Pts',(4.78731129503681,0.205616875855751,3.41573023112194));
#21800=CARTESIAN_POINT('Ctrl Pts',(4.81116921306823,0.460426689658758,3.5856852332931));
#21801=CARTESIAN_POINT('Ctrl Pts',(4.83502713109965,0.60264963606909,3.85695148163183));
#21802=CARTESIAN_POINT('Ctrl Pts',(4.85888504913107,0.597508330613982,4.16319698927494));
#21803=CARTESIAN_POINT('Ctrl Pts',(4.88274296716248,0.446259962523644,4.42953638764361));
#21804=CARTESIAN_POINT('Ctrl Pts',(4.90660088519391,0.185888877718945,4.59084243889714));
#21805=CARTESIAN_POINT('Ctrl Pts',(4.93045880322533,-0.119937101199393,
4.60767141961541));
#21806=CARTESIAN_POINT('Ctrl Pts',(4.95431672125674,-0.396435191853442,
4.47590818560059));
#21807=CARTESIAN_POINT('Ctrl Pts',(4.97817463928816,-0.575994079421511,
4.22777243672773));
#21808=CARTESIAN_POINT('Ctrl Pts',(5.00203255731958,-0.614706724807315,
3.92394012267834));
#21809=CARTESIAN_POINT('Ctrl Pts',(5.025890475351,-0.503106831702736,3.63870652046354));
#21810=CARTESIAN_POINT('Ctrl Pts',(5.04974839338242,-0.268483613891896,
3.44181901543221));
#21811=CARTESIAN_POINT('Ctrl Pts',(5.07360631141384,0.0317911608623165,
3.38142196567243));
#21812=CARTESIAN_POINT('Ctrl Pts',(5.09746422944526,0.32429213081186,3.47228409503311));
#21813=CARTESIAN_POINT('Ctrl Pts',(5.12132214747667,0.537494841237617,3.69218713785082));
#21814=CARTESIAN_POINT('Ctrl Pts',(5.1451800655081,0.619265421915264,3.98735881011802));
#21815=CARTESIAN_POINT('Ctrl Pts',(5.16903798353952,0.549608738483219,4.28562159765047));
#21816=CARTESIAN_POINT('Ctrl Pts',(5.19289590157094,0.34555774745058,4.51404212438126));
#21817=CARTESIAN_POINT('Ctrl Pts',(5.21675381960235,0.0570084743622218,
4.61676534947452));
#21818=CARTESIAN_POINT('Ctrl Pts',(5.24061173763377,-0.245480923587363,
4.56867264627043));
#21819=CARTESIAN_POINT('Ctrl Pts',(5.26446965566519,-0.487943548953736,
4.38152399072137));
#21820=CARTESIAN_POINT('Ctrl Pts',(5.28832757369661,-0.611090685285508,
4.10108232693608));
#21821=CARTESIAN_POINT('Ctrl Pts',(5.31218549172803,-0.584809503288917,
3.79592328078761));
#21822=CARTESIAN_POINT('Ctrl Pts',(5.33604340975945,-0.415526467847156,
3.5406665514248));
#21823=CARTESIAN_POINT('Ctrl Pts',(5.35990132779088,-0.144635892303038,
3.39772936223054));
#21824=CARTESIAN_POINT('Ctrl Pts',(5.38375924582228,0.161622098711782,3.40206374949372));
#21825=CARTESIAN_POINT('Ctrl Pts',(5.40761716385371,0.428359084093981,3.55260983746209));
#21826=CARTESIAN_POINT('Ctrl Pts',(5.43147508188512,0.590350605148055,3.81255500683439));
#21827=CARTESIAN_POINT('Ctrl Pts',(5.45533299991655,0.607985322415754,4.11833558293467));
#21828=CARTESIAN_POINT('Ctrl Pts',(5.47919091794796,0.476951067165249,4.39517988561105));
#21829=CARTESIAN_POINT('Ctrl Pts',(5.50304883597938,0.2292892841064,4.57539194177126));
#21830=CARTESIAN_POINT('Ctrl Pts',(5.5269067540108,-0.0744399746307492,
4.61490499480714));
#21831=CARTESIAN_POINT('Ctrl Pts',(5.55076467204222,-0.359966631867259,
4.5040570269359));
#21832=CARTESIAN_POINT('Ctrl Pts',(5.57462259007364,-0.55747164231658,4.26995338574299));
#21833=CARTESIAN_POINT('Ctrl Pts',(5.59848050810506,-0.618659650999605,
3.96983878834977));
#21834=CARTESIAN_POINT('Ctrl Pts',(5.62233842613648,-0.528568523057477,
3.67709942878664));
#21835=CARTESIAN_POINT('Ctrl Pts',(5.6461963441679,-0.309227993320144,3.46331805450751));
#21836=CARTESIAN_POINT('Ctrl Pts',(5.67005426219932,-0.0142727959960426,
3.38077003484781));
#21837=CARTESIAN_POINT('Ctrl Pts',(5.69391218023074,0.284172488697173,3.4496406091084));
#21838=CARTESIAN_POINT('Ctrl Pts',(5.71777009826216,0.513129859266986,3.65308904601577));
#21839=CARTESIAN_POINT('Ctrl Pts',(5.74162801629357,0.616613001744231,3.94136666067651));
#21840=CARTESIAN_POINT('Ctrl Pts',(5.765485934325,0.569317469330215,4.24398172424487));
#21841=CARTESIAN_POINT('Ctrl Pts',(5.78934385235641,0.382808307322586,4.48693660973462));
#21842=CARTESIAN_POINT('Ctrl Pts',(5.81320177038783,0.102692087527565,4.61082223133738));
#21843=CARTESIAN_POINT('Ctrl Pts',(5.83705968841925,-0.202535146533943,
4.58534517687525));
#21844=CARTESIAN_POINT('Ctrl Pts',(5.86091760645067,-0.458237017319611,
4.41673528603543));
#21845=CARTESIAN_POINT('Ctrl Pts',(5.88477552448209,-0.601887460912657,
4.14622225884759));
#21846=CARTESIAN_POINT('Ctrl Pts',(5.9086334425135,-0.598360014525416,3.83995392008642));
#21847=CARTESIAN_POINT('Ctrl Pts',(5.93249136054493,-0.448517265794504,
3.57282118150817));
#21848=CARTESIAN_POINT('Ctrl Pts',(5.95634927857635,-0.188999790056246,
3.41014534911766));
#21849=CARTESIAN_POINT('Ctrl Pts',(5.98020719660777,0.116733210556207,3.39170495376011));
#21850=CARTESIAN_POINT('Ctrl Pts',(6.00406511463918,0.393921897475357,3.52200944135141));
#21851=CARTESIAN_POINT('Ctrl Pts',(6.02792303267061,0.574785693380153,3.76919531120668));
#21852=CARTESIAN_POINT('Ctrl Pts',(6.05178095070201,0.61509921541814,4.07281983667942));
#21853=CARTESIAN_POINT('Ctrl Pts',(6.07563886873346,0.505003308517799,4.35863675364492));
#21854=CARTESIAN_POINT('Ctrl Pts',(6.09949678676485,0.27142206589204,4.55675943366228));
#21855=CARTESIAN_POINT('Ctrl Pts',(6.12335470479629,-0.0285325303540597,
4.61873507756083));
#21856=CARTESIAN_POINT('Ctrl Pts',(6.14721262282769,-0.321503980505702,
4.52942105023226));
#21857=CARTESIAN_POINT('Ctrl Pts',(6.17107054085913,-0.535870591003297,
4.31063422072759));
#21858=CARTESIAN_POINT('Ctrl Pts',(6.19492845889052,-0.619180264299368,
4.01591706164003));
#21859=CARTESIAN_POINT('Ctrl Pts',(6.21878637692196,-0.551125001039776,
3.71725450231754));
#21860=CARTESIAN_POINT('Ctrl Pts',(6.24264429495337,-0.348226295733882,
3.48783145534908));
#21861=CARTESIAN_POINT('Ctrl Pts',(6.2665022129848,-0.0603247367796791,
3.38345774569467));
#21862=CARTESIAN_POINT('Ctrl Pts',(6.29036013101621,0.242607149567705,3.43020375417728));
#21863=CARTESIAN_POINT('Ctrl Pts',(6.31421804904763,0.485688404846908,3.61560451082823));
#21864=CARTESIAN_POINT('Ctrl Pts',(6.33807596707905,0.61099356578022,3.89627130770405));
#21865=CARTESIAN_POINT('Ctrl Pts',(6.36193388511046,0.585080291527744,4.19994745529594));
#21866=CARTESIAN_POINT('Ctrl Pts',(6.3937444424857,0.363797450650833,4.54512657044717));
#21867=CARTESIAN_POINT('Ctrl Pts',(6.43350763920472,-0.178959141669374,
4.67939801199369));
#21868=CARTESIAN_POINT('Ctrl Pts',(6.48122347526757,-0.668951848353412,
4.21606826543601));
#21869=CARTESIAN_POINT('Ctrl Pts',(6.5289393113304,-0.543175254381078,3.55462676401443));
#21870=CARTESIAN_POINT('Ctrl Pts',(6.57665514739324,0.0806513803028556,
3.30201433154981));
#21871=CARTESIAN_POINT('Ctrl Pts',(6.62437098345608,0.630812951656228,3.69045991683978));
#21872=CARTESIAN_POINT('Ctrl Pts',(6.67208681951892,0.601478580142798,4.36311480674272));
#21873=CARTESIAN_POINT('Ctrl Pts',(6.71980265558175,0.0199087309838695,
4.70234020845997));
#21874=CARTESIAN_POINT('Ctrl Pts',(6.76751849164459,-0.580002689552455,
4.39658285339385));
#21875=CARTESIAN_POINT('Ctrl Pts',(6.81523432770743,-0.64725742864426,3.72664421308375));
#21876=CARTESIAN_POINT('Ctrl Pts',(6.86295016377027,-0.120142281411799,
3.30772876957018));
#21877=CARTESIAN_POINT('Ctrl Pts',(6.91066599983311,0.517310146858294,3.52453857056345));
#21878=CARTESIAN_POINT('Ctrl Pts',(6.95838183589594,0.679704059947864,4.17797090041396));
#21879=CARTESIAN_POINT('Ctrl Pts',(7.00609767195879,0.217917737520193,4.66797035296266));
#21880=CARTESIAN_POINT('Ctrl Pts',(7.05381350802161,-0.443987099894697,
4.54456206689342));
#21881=CARTESIAN_POINT('Ctrl Pts',(7.10152934408447,-0.698171061503544,
3.92107420680554));
#21882=CARTESIAN_POINT('Ctrl Pts',(7.14924518014729,-0.311214160204793,
3.3700650369752));
#21883=CARTESIAN_POINT('Ctrl Pts',(7.19696101621015,0.361535686685884,3.39753487888718));
#21884=CARTESIAN_POINT('Ctrl Pts',(7.24467685227297,0.702281647003851,3.97825768917858));
#21885=CARTESIAN_POINT('Ctrl Pts',(7.29239268833582,0.398111619195611,4.5789468099385));
#21886=CARTESIAN_POINT('Ctrl Pts',(7.34010852439865,-0.271650463017158,
4.64798016059173));
#21887=CARTESIAN_POINT('Ctrl Pts',(7.38782436046149,-0.691951729928866,
4.1219633626529));
#21888=CARTESIAN_POINT('Ctrl Pts',(7.43554019652432,-0.476823084268312,
3.48394573037578));
#21889=CARTESIAN_POINT('Ctrl Pts',(7.48325603258717,0.17617954081454,3.31982867534575));
#21890=CARTESIAN_POINT('Ctrl Pts',(7.53097186865001,0.667393780433987,3.78032341303133));
#21891=CARTESIAN_POINT('Ctrl Pts',(7.57868770471284,0.545730043505963,4.44255054095139));
#21892=CARTESIAN_POINT('Ctrl Pts',(7.62640354077568,-0.077085990144297,
4.69837669746149));
#21893=CARTESIAN_POINT('Ctrl Pts',(7.67411937683852,-0.629112772588521,
4.31287278685955));
#21894=CARTESIAN_POINT('Ctrl Pts',(7.72183521290136,-0.603415615998442,
3.64005298187887));
#21895=CARTESIAN_POINT('Ctrl Pts',(7.76955104896419,-0.0235926144000291,
3.29777806215626));
#21896=CARTESIAN_POINT('Ctrl Pts',(7.81726688502703,0.577895847971041,3.60036435301798));
#21897=CARTESIAN_POINT('Ctrl Pts',(7.86498272108987,0.648693661106154,4.26994220769392));
#21898=CARTESIAN_POINT('Ctrl Pts',(7.9126985571527,0.123786103798515,4.6916279794467));
#21899=CARTESIAN_POINT('Ctrl Pts',(7.96041439321555,-0.514796137313916,
4.47818113561083));
#21900=CARTESIAN_POINT('Ctrl Pts',(8.00813022927838,-0.680633164378164,
3.82561319718015));
#21901=CARTESIAN_POINT('Ctrl Pts',(8.05584606534123,-0.221434283704469,
3.33318734306526));
#21902=CARTESIAN_POINT('Ctrl Pts',(8.10356190140405,0.441111106898351,3.45310581204486));
#21903=CARTESIAN_POINT('Ctrl Pts',(8.1512777374669,0.698577380670183,4.07524562887252));
#21904=CARTESIAN_POINT('Ctrl Pts',(8.19899357352974,0.314529296777622,4.62828622690367));
#21905=CARTESIAN_POINT('Ctrl Pts',(8.24670940959258,-0.358355880000973,
4.60436191534297));
#21906=CARTESIAN_POINT('Ctrl Pts',(8.29442524565541,-0.70215733816079,4.02544275761943));
#21907=CARTESIAN_POINT('Ctrl Pts',(8.34214108171825,-0.401156908608127,
3.42315912408683));
#21908=CARTESIAN_POINT('Ctrl Pts',(8.3898569177811,0.268232082711808,3.35059734274305));
#21909=CARTESIAN_POINT('Ctrl Pts',(8.43757275384392,0.691299425196396,3.8743920139026));
#21910=CARTESIAN_POINT('Ctrl Pts',(8.48528858990677,0.479535868514212,4.51353443142269));
#21911=CARTESIAN_POINT('Ctrl Pts',(8.53300442596961,-0.172592854832336,
4.68109027882443));
#21912=CARTESIAN_POINT('Ctrl Pts',(8.58072026203244,-0.66622690390392,4.22319044326068));
#21913=CARTESIAN_POINT('Ctrl Pts',(8.62843609809529,-0.548054535901959,
3.56033138942427));
#21914=CARTESIAN_POINT('Ctrl Pts',(8.67615193415812,0.0734047453217555,
3.30122678585069));
#21915=CARTESIAN_POINT('Ctrl Pts',(8.72386777022095,0.627455319439314,3.68381637683837));
#21916=CARTESIAN_POINT('Ctrl Pts',(8.7715836062838,0.605304019074675,4.35676225408577));
#21917=CARTESIAN_POINT('Ctrl Pts',(8.81929944234663,0.0272927241942496,
4.70208786391332));
#21918=CARTESIAN_POINT('Ctrl Pts',(8.86701527840948,-0.575781899266294,
4.40267538529889));
#21919=CARTESIAN_POINT('Ctrl Pts',(8.9147311144723,-0.650107145087294,3.73347990440727));
#21920=CARTESIAN_POINT('Ctrl Pts',(8.96244695053515,-0.127428996390418,
3.30903392823725));
#21921=CARTESIAN_POINT('Ctrl Pts',(9.01016278659798,0.512269160438921,3.51911272764658));
#21922=CARTESIAN_POINT('Ctrl Pts',(9.05787862266082,0.681542664962993,4.17079770865984));
#21923=CARTESIAN_POINT('Ctrl Pts',(9.10559445872366,0.224945053369686,4.66563652575022));
#21924=CARTESIAN_POINT('Ctrl Pts',(9.1533102947865,-0.438223061957547,4.54921107910972));
#21925=CARTESIAN_POINT('Ctrl Pts',(9.20102613084934,-0.698964196560635,
3.92843664782408));
#21926=CARTESIAN_POINT('Ctrl Pts',(9.24874196691217,-0.317835754515511,
3.3733799439853));
#21927=CARTESIAN_POINT('Ctrl Pts',(9.29645780297501,0.355166151432911,3.39375807937372));
#21928=CARTESIAN_POINT('Ctrl Pts',(9.34417363903786,0.702013515586798,3.97085749870423));
#21929=CARTESIAN_POINT('Ctrl Pts',(9.39188947510068,0.404191066510942,4.57471892538967));
#21930=CARTESIAN_POINT('Ctrl Pts',(9.43960531116354,-0.264806258220881,
4.65080711970243));
#21931=CARTESIAN_POINT('Ctrl Pts',(9.48732114722635,-0.690627921460452,
4.12924912203773));
#21932=CARTESIAN_POINT('Ctrl Pts',(9.53503698328922,-0.482235337746388,
3.48899966685243));
#21933=CARTESIAN_POINT('Ctrl Pts',(9.58275281935202,0.169001376764621,3.31800968034731));
#21934=CARTESIAN_POINT('Ctrl Pts',(9.63046865541491,0.665041526572246,3.77330189814918));
#21935=CARTESIAN_POINT('Ctrl Pts',(9.6781844914777,0.550363809549371,4.43677447107931));
#21936=CARTESIAN_POINT('Ctrl Pts',(9.72590032754056,-0.0697214622184181,
4.69915032657822));
#21937=CARTESIAN_POINT('Ctrl Pts',(9.7736161636034,-0.625780442428439,4.31948567936979));
#21938=CARTESIAN_POINT('Ctrl Pts',(9.82133199966623,-0.607175613486645,
3.64643241687702));
#21939=CARTESIAN_POINT('Ctrl Pts',(9.86904783572907,-0.030992076082374,
3.29806570630264));
#21940=CARTESIAN_POINT('Ctrl Pts',(9.91676367179191,0.573651961662729,3.59429605827795));
#21941=CARTESIAN_POINT('Ctrl Pts',(9.96447950785474,0.651502576242943,4.26309058249416));
#21942=CARTESIAN_POINT('Ctrl Pts',(10.0121953439176,0.131068350403577,4.69028497663703));
#21943=CARTESIAN_POINT('Ctrl Pts',(10.0599111799804,-0.50972795835719,4.48358005533451));
#21944=CARTESIAN_POINT('Ctrl Pts',(10.1076270160433,-0.682433239785766,
3.83279612838271));
#21945=CARTESIAN_POINT('Ctrl Pts',(10.1553428521061,-0.228449576533966,
3.33555808949935));
#21946=CARTESIAN_POINT('Ctrl Pts',(10.2030586881689,0.435322847997542,3.44848728078164));
#21947=CARTESIAN_POINT('Ctrl Pts',(10.2507745242318,0.699331602909907,4.06787908823615));
#21948=CARTESIAN_POINT('Ctrl Pts',(10.2984903602946,0.321133386270249,4.62493648450936));
#21949=CARTESIAN_POINT('Ctrl Pts',(10.3462061963575,-0.351966560253669,
4.60810509117381));
#21950=CARTESIAN_POINT('Ctrl Pts',(10.3939220324203,-0.701850198794989,
4.03284143571381));
#21951=CARTESIAN_POINT('Ctrl Pts',(10.4416378684831,-0.407214000429435,
3.42741898450738));
#21952=CARTESIAN_POINT('Ctrl Pts',(10.489353704546,0.261373080323254,3.34780649011919));
#21953=CARTESIAN_POINT('Ctrl Pts',(10.5370695406088,0.689937239673316,3.86711333114163));
#21954=CARTESIAN_POINT('Ctrl Pts',(10.5847853766716,0.484921415782374,4.50845204490092));
#21955=CARTESIAN_POINT('Ctrl Pts',(10.6325012127345,-0.165405205696588,
4.68287142228737));
#21956=CARTESIAN_POINT('Ctrl Pts',(10.6802170487973,-0.66383768169814,4.23019946525991));
#21957=CARTESIAN_POINT('Ctrl Pts',(10.7279328848602,-0.552657800140614,
3.5661317972102));
#21958=CARTESIAN_POINT('Ctrl Pts',(10.775648720923,0.0660362430193439,3.30049197570278));
#21959=CARTESIAN_POINT('Ctrl Pts',(10.8233645569858,0.624088188116435,3.67722113622194));
#21960=CARTESIAN_POINT('Ctrl Pts',(10.8710803930487,0.609030347235101,4.3503630939397));
#21961=CARTESIAN_POINT('Ctrl Pts',(10.9187962291115,0.0346905673513346,
4.70176123146349));
#21962=CARTESIAN_POINT('Ctrl Pts',(10.9665120651743,-0.57150609431415,4.40872123214985));
#21963=CARTESIAN_POINT('Ctrl Pts',(11.0142279012372,-0.65287991581936,3.74034623636848));
#21964=CARTESIAN_POINT('Ctrl Pts',(11.0619437373,-0.134704064778877,3.31041528701663));
#21965=CARTESIAN_POINT('Ctrl Pts',(11.1096595733629,0.507172601636502,3.51374059022208));
#21966=CARTESIAN_POINT('Ctrl Pts',(11.1573754094257,0.68330486411552,4.16360539148934));
#21967=CARTESIAN_POINT('Ctrl Pts',(11.2050912454885,0.231947755880478,4.66322884435941));
#21968=CARTESIAN_POINT('Ctrl Pts',(11.2528070815514,-0.432410545554582,
4.55379904436673));
#21969=CARTESIAN_POINT('Ctrl Pts',(11.3005229176142,-0.699679589515398,
3.93580706063847));
#21970=CARTESIAN_POINT('Ctrl Pts',(11.348238753677,-0.324422100469907,3.37676444086124));
#21971=CARTESIAN_POINT('Ctrl Pts',(11.3959545897399,0.348757195312759,3.39004862475285));
#21972=CARTESIAN_POINT('Ctrl Pts',(11.4436704258027,0.701667392320496,3.9634605418422));
#21973=CARTESIAN_POINT('Ctrl Pts',(11.4913862618656,0.410225626419724,4.57042720558968));
#21974=CARTESIAN_POINT('Ctrl Pts',(11.5391020979284,-0.257932644354891,
4.65356178929341));
#21975=CARTESIAN_POINT('Ctrl Pts',(11.5868179339912,-0.689227399014534,
4.13652052554825));
#21976=CARTESIAN_POINT('Ctrl Pts',(11.6345337700541,-0.487594028032435,
3.49411036255383));
#21977=CARTESIAN_POINT('Ctrl Pts',(11.6822496061169,0.161804441490335,3.31626643773886));
#21978=CARTESIAN_POINT('Ctrl Pts',(11.7299654421798,0.662615402711184,3.76630556374144));
#21979=CARTESIAN_POINT('Ctrl Pts',(11.7776812782426,0.554936443973853,4.43094988641136));
#21980=CARTESIAN_POINT('Ctrl Pts',(11.8253971143054,-0.062349190059417,
4.69984629737339));
#21981=CARTESIAN_POINT('Ctrl Pts',(11.8731129503683,-0.622378603495518,
4.32606308493799));
#21982=CARTESIAN_POINT('Ctrl Pts',(11.9208287864311,-0.610868168815925,
3.65285112447858));
#21983=CARTESIAN_POINT('Ctrl Pts',(11.9685446224939,-0.0383880952977111,
3.29843131798253));
#21984=CARTESIAN_POINT('Ctrl Pts',(12.0162604585568,0.569344356809164,3.58827282720487));
#21985=CARTESIAN_POINT('Ctrl Pts',(12.0639762946196,0.654239125569198,4.25620973444184));
#21986=CARTESIAN_POINT('Ctrl Pts',(12.1116921306825,0.138336038556134,4.68886530024737));
#21987=CARTESIAN_POINT('Ctrl Pts',(12.1594079667453,-0.50460316123658,4.48892526128066));
#21988=CARTESIAN_POINT('Ctrl Pts',(12.2071238028081,-0.684157513748105,
3.83999763179777));
#21989=CARTESIAN_POINT('Ctrl Pts',(12.254839638871,-0.235439494268261,3.33800263898788));
#21990=CARTESIAN_POINT('Ctrl Pts',(12.3025554749338,0.429486235500398,3.44393000893412));
#21991=CARTESIAN_POINT('Ctrl Pts',(12.3502713109967,0.700008146713868,4.06050500791278));
#21992=CARTESIAN_POINT('Ctrl Pts',(12.3979871470595,0.327701805790174,4.62151732713591));
#21993=CARTESIAN_POINT('Ctrl Pts',(12.4457029831223,-0.345538145731053,
4.61178072157682));
#21994=CARTESIAN_POINT('Ctrl Pts',(12.4934188191852,-0.701465101239671,
4.04023646593735));
#21995=CARTESIAN_POINT('Ctrl Pts',(12.541134655248,-0.413225860851952,3.43174244451));
#21996=CARTESIAN_POINT('Ctrl Pts',(12.5888504913108,0.254485045853264,3.34508808005552));
#21997=CARTESIAN_POINT('Ctrl Pts',(12.6365663273737,0.688498419195676,3.85984940880123));
#21998=CARTESIAN_POINT('Ctrl Pts',(12.6842821634365,0.490253100280801,4.50331318193882));
#21999=CARTESIAN_POINT('Ctrl Pts',(12.7319979994994,-0.158199184135511,
4.68457671563321));
#22000=CARTESIAN_POINT('Ctrl Pts',(12.7797138355622,-0.661374723552845,
4.23718291779492));
#22001=CARTESIAN_POINT('Ctrl Pts',(12.827429671625,-0.557199677773407,3.57198039701723));
#22002=CARTESIAN_POINT('Ctrl Pts',(12.8751455076879,0.058660405724426,3.29983486358678));
#22003=CARTESIAN_POINT('Ctrl Pts',(12.9228613437507,0.62065173603916,3.67066174834999));
#22004=CARTESIAN_POINT('Ctrl Pts',(12.9705771798135,0.612689027194643,4.34392501712378));
#22005=CARTESIAN_POINT('Ctrl Pts',(13.0182930158764,0.0420845572448178,
4.7013566507062));
#22006=CARTESIAN_POINT('Ctrl Pts',(13.0660088519392,-0.567166809177069,
4.4147216801859));
#22007=CARTESIAN_POINT('Ctrl Pts',(13.1137246880021,-0.655580167748548,
3.74724140943759));
#22008=CARTESIAN_POINT('Ctrl Pts',(13.1614405240649,-0.141964170879043,
3.31187324159358));
#22009=CARTESIAN_POINT('Ctrl Pts',(13.2091563601277,0.502019708508231,3.50842246418533));
#22010=CARTESIAN_POINT('Ctrl Pts',(13.2568721961906,0.684991165006287,4.15639490180834));
#22011=CARTESIAN_POINT('Ctrl Pts',(13.3045880322534,0.238924694735218,4.66074749465585));
#22012=CARTESIAN_POINT('Ctrl Pts',(13.3523038683163,-0.426549999040181,
4.55832549625387));
#22013=CARTESIAN_POINT('Ctrl Pts',(13.4000197043791,-0.700317265381609,
3.94318460369993));
#22014=CARTESIAN_POINT('Ctrl Pts',(13.4477355404419,-0.330972411156884,
3.38021816378559));
#22015=CARTESIAN_POINT('Ctrl Pts',(13.4954513765048,0.342309500898352,3.3864069206363));
#22016=CARTESIAN_POINT('Ctrl Pts',(13.5431672125676,0.70124333116994,3.95606764360979));
#22017=CARTESIAN_POINT('Ctrl Pts',(13.5908830486304,0.416214620412595,4.5660721254426));
#22018=CARTESIAN_POINT('Ctrl Pts',(13.6385988846933,-0.251030380554765,
4.65624386434224));
#22019=CARTESIAN_POINT('Ctrl Pts',(13.6863147207561,-0.687750320459788,
4.14377676500662));
#22020=CARTESIAN_POINT('Ctrl Pts',(13.734030556819,-0.492898558687668,3.49927725007553));
#22021=CARTESIAN_POINT('Ctrl Pts',(13.7817463928818,0.15458953374652,3.31459914100992));
#22022=CARTESIAN_POINT('Ctrl Pts',(13.8294622289446,0.660115678675556,3.75933518700271));
#22023=CARTESIAN_POINT('Ctrl Pts',(13.8771780650075,0.559447438691528,4.42507743387505));
#22024=CARTESIAN_POINT('Ctrl Pts',(13.9248939010703,-0.0549699924482557,
4.7004645325629));
#22025=CARTESIAN_POINT('Ctrl Pts',(13.9726097371331,-0.61890763370075,4.33260427296601));
#22026=CARTESIAN_POINT('Ctrl Pts',(14.020325573196,-0.614492871807821,3.65930839172987));
#22027=CARTESIAN_POINT('Ctrl Pts',(14.0680414092588,-0.0457798505455885,
3.29887485658241));
#22028=CARTESIAN_POINT('Ctrl Pts',(14.1157572453217,0.564973511886205,3.58229532883235));
#22029=CARTESIAN_POINT('Ctrl Pts',(14.1634730813845,0.656903005118004,4.24930042782804));
#22030=CARTESIAN_POINT('Ctrl Pts',(14.2111889174473,0.145588360997982,4.6873691079691));
#22031=CARTESIAN_POINT('Ctrl Pts',(14.2589047535102,-0.499422315191365,
4.49421615972892));
#22032=CARTESIAN_POINT('Ctrl Pts',(14.306620589573,-0.685805794740406,3.8472169075166));
#22033=CARTESIAN_POINT('Ctrl Pts',(14.3543364256359,-0.242403260500786,
3.34052072000184));
#22034=CARTESIAN_POINT('Ctrl Pts',(14.4020522616987,0.423601917710294,3.43943450270243));
#22035=CARTESIAN_POINT('Ctrl Pts',(14.4497680977615,0.700606936934704,4.05312420698026));
#22036=CARTESIAN_POINT('Ctrl Pts',(14.4974839338244,0.334233825748585,4.61802913456711));
#22037=CARTESIAN_POINT('Ctrl Pts',(14.5451997698872,-0.339071350470923,
4.61538839828042));
#22038=CARTESIAN_POINT('Ctrl Pts',(14.59291560595,-0.701002088269634,4.04762702688518));
#22039=CARTESIAN_POINT('Ctrl Pts',(14.6406314420129,-0.419191822106764,
3.43612902386528));
#22040=CARTESIAN_POINT('Ctrl Pts',(14.6883472780757,0.24756874439201,3.34244241450009));
#22041=CARTESIAN_POINT('Ctrl Pts',(14.7360631141386,0.686983123580828,3.85260105372344));
#22042=CARTESIAN_POINT('Ctrl Pts',(14.7837789502014,0.495530329791292,4.49811841333687));
#22043=CARTESIAN_POINT('Ctrl Pts',(14.8314947862642,-0.150975590559777,
4.68620596944608));
#22044=CARTESIAN_POINT('Ctrl Pts',(14.8792106223271,-0.658838303041738,
4.24414002517693));
#22045=CARTESIAN_POINT('Ctrl Pts',(14.9269264583899,-0.561679664310124,
3.57787653921065));
#22046=CARTESIAN_POINT('Ctrl Pts',(14.9746422944528,0.0512780527100071,
3.29925552249156));
#22047=CARTESIAN_POINT('Ctrl Pts',(15.0223581305156,0.617146344912281,3.6641389418082));
#22048=CARTESIAN_POINT('Ctrl Pts',(15.0700739665784,0.616279652564493,4.337448738749));
#22049=CARTESIAN_POINT('Ctrl Pts',(15.1177898026413,0.0494738725853903,
4.70087416658037));
#22050=CARTESIAN_POINT('Ctrl Pts',(15.1655056387041,-0.562764525842253,
4.42067606290572));
#22051=CARTESIAN_POINT('Ctrl Pts',(15.2132214747669,-0.658207600943685,
3.75416465773151));
#22052=CARTESIAN_POINT('Ctrl Pts',(15.2609373108298,-0.14920850827279,3.31340763002542));
#22053=CARTESIAN_POINT('Ctrl Pts',(15.3086531468926,0.496811053413015,3.50315894024854));
#22054=CARTESIAN_POINT('Ctrl Pts',(15.3563689829554,0.686601380328997,4.14916704052379));
#22055=CARTESIAN_POINT('Ctrl Pts',(15.4040848190183,0.245875094968658,4.6581927522561));
#22056=CARTESIAN_POINT('Ctrl Pts',(15.4518006550811,-0.420642073376032,
4.56278993199436));
#22057=CARTESIAN_POINT('Ctrl Pts',(15.499516491144,-0.700877153329261,3.95056845754601));
#22058=CARTESIAN_POINT('Ctrl Pts',(15.5472323272068,-0.337485958999024,
3.3837407291352));
#22059=CARTESIAN_POINT('Ctrl Pts',(15.5949481632696,0.335823784368978,3.38283337152726));
#22060=CARTESIAN_POINT('Ctrl Pts',(15.6426639993325,0.70074137923783,3.94867962517506));
#22061=CARTESIAN_POINT('Ctrl Pts',(15.6903798353953,0.422157383260532,4.56165416869007));
#22062=CARTESIAN_POINT('Ctrl Pts',(15.7380956714582,-0.244100233491204,
4.65885304693675));
#22063=CARTESIAN_POINT('Ctrl Pts',(15.785811507521,-0.686196849863089,4.15101703442422));
#22064=CARTESIAN_POINT('Ctrl Pts',(15.8335273435838,-0.498148340509996,
3.50449975550414));
#22065=CARTESIAN_POINT('Ctrl Pts',(15.8812431796467,0.147357454930898,3.3130079753559));
#22066=CARTESIAN_POINT('Ctrl Pts',(15.9289590157095,0.657542632122849,3.75239154216938));
#22067=CARTESIAN_POINT('Ctrl Pts',(15.9766748517723,0.563896292642505,4.41915776575455));
#22068=CARTESIAN_POINT('Ctrl Pts',(16.0243906878352,-0.0475846890311933,
4.70100496347609));
#22069=CARTESIAN_POINT('Ctrl Pts',(16.072106523898,-0.615367918582998,4.33910851688972));
#22070=CARTESIAN_POINT('Ctrl Pts',(16.1198223599609,-0.618049319847516,
3.66580350138828));
#22071=CARTESIAN_POINT('Ctrl Pts',(16.1675381960237,-0.0531665207849041,
3.29939627283611));
#22072=CARTESIAN_POINT('Ctrl Pts',(16.2152540320865,0.560539912386559,3.57636422711252));
#22073=CARTESIAN_POINT('Ctrl Pts',(16.2629698681494,0.659493918998266,4.24236343010572));
#22074=CARTESIAN_POINT('Ctrl Pts',(16.3106857042122,0.152824512175573,4.68579656599215));
#22075=CARTESIAN_POINT('Ctrl Pts',(16.358401540275,-0.494185995685336,4.49945216299141));
#22076=CARTESIAN_POINT('Ctrl Pts',(16.4061173763379,-0.687377899679438,
3.85445315365633));
#22077=CARTESIAN_POINT('Ctrl Pts',(16.4538332124007,-0.249340101729437,
3.34311205284473));
#22078=CARTESIAN_POINT('Ctrl Pts',(16.5015490484636,0.417670548229327,3.43500126142608));
#22079=CARTESIAN_POINT('Ctrl Pts',(16.5492648845264,0.701127907061643,4.04573750526291));
#22080=CARTESIAN_POINT('Ctrl Pts',(16.5969807205892,0.340728720599694,4.61447229425484));
#22081=CARTESIAN_POINT('Ctrl Pts',(16.6446965566521,-0.3325668927742,4.61892772056098));
#22082=CARTESIAN_POINT('Ctrl Pts',(16.6924123927149,-0.700461211314163,
4.05501229764889));
#22083=CARTESIAN_POINT('Ctrl Pts',(16.7401282287777,-0.425111221523205,
3.4405782353328));
#22084=CARTESIAN_POINT('Ctrl Pts',(16.7878440648406,0.240624944169445,3.3398697873209));
#22085=CARTESIAN_POINT('Ctrl Pts',(16.8355599009034,0.685391521140609,3.84536907102113));
#22086=CARTESIAN_POINT('Ctrl Pts',(16.8832757369663,0.500752518144239,4.49286831610534));
#22087=CARTESIAN_POINT('Ctrl Pts',(16.9309915730291,-0.143735227331884,
4.68775900275617));
#22088=CARTESIAN_POINT('Ctrl Pts',(16.978707409092,-0.656228701898373,4.25107001464348));
#22089=CARTESIAN_POINT('Ctrl Pts',(17.0264232451548,-0.566097262135119,
3.58381956887496));
#22090=CARTESIAN_POINT('Ctrl Pts',(17.0741390812176,0.0438900039728252,
3.29875401676759));
#22091=CARTESIAN_POINT('Ctrl Pts',(17.1218549172805,0.613572404098014,3.65765344111895));
#22092=CARTESIAN_POINT('Ctrl Pts',(17.1695707533433,0.619801824515016,4.33093497816967));
#22093=CARTESIAN_POINT('Ctrl Pts',(17.2172865894061,0.0568576926029748,
4.70031383267802));
#22094=CARTESIAN_POINT('Ctrl Pts',(17.265002425469,-0.558299733294432,4.42658371892475));
#22095=CARTESIAN_POINT('Ctrl Pts',(17.3127182615318,-0.66076192356197,3.76111521224867));
#22096=CARTESIAN_POINT('Ctrl Pts',(17.3604340975947,-0.156436272293483,
3.31501828187956));
#22097=CARTESIAN_POINT('Ctrl Pts',(17.4081499336575,0.491547214903555,3.49795060305896));
#22098=CARTESIAN_POINT('Ctrl Pts',(17.4558657697204,0.688135331228569,4.14192261047223));
#22099=CARTESIAN_POINT('Ctrl Pts',(17.5035816057831,0.252798184563325,4.65556490092881));
#22100=CARTESIAN_POINT('Ctrl Pts',(17.551297441846,-0.414687424786488,4.56719185569987));
#22101=CARTESIAN_POINT('Ctrl Pts',(17.5990132779088,-0.701359191168653,
3.95795780201324));
#22102=CARTESIAN_POINT('Ctrl Pts',(17.6467291139717,-0.343962020502345,
3.38733174564023));
#22103=CARTESIAN_POINT('Ctrl Pts',(17.6944449500345,0.329300766127249,3.37932837435862));
#22104=CARTESIAN_POINT('Ctrl Pts',(17.7421607860974,0.700161592278611,3.94129730716402));
#22105=CARTESIAN_POINT('Ctrl Pts',(17.7898766221602,0.428053254869629,4.55717382605774));
#22106=CARTESIAN_POINT('Ctrl Pts',(17.837592458223,-0.23714297293205,4.66138904726133));
#22107=CARTESIAN_POINT('Ctrl Pts',(17.8853082942859,-0.684567159776581,
4.15824052958626));
#22108=CARTESIAN_POINT('Ctrl Pts',(17.9330241303487,-0.503342790378573,
3.50977729874859));
#22109=CARTESIAN_POINT('Ctrl Pts',(17.9807399664116,0.140109008348428,3.31149311751593));
#22110=CARTESIAN_POINT('Ctrl Pts',(18.0284558024744,0.654896548854854,3.7454754005085));
#22111=CARTESIAN_POINT('Ctrl Pts',(18.0761716385372,0.568282511669218,4.41319153957849));
#22112=CARTESIAN_POINT('Ctrl Pts',(18.1238874746001,-0.040194100132671,
4.70146753008449));
#22113=CARTESIAN_POINT('Ctrl Pts',(18.1716033106629,-0.611759851316993,
4.34557509424858));
#22114=CARTESIAN_POINT('Ctrl Pts',(18.2193191467258,-0.621537117901666,
3.67233573200791));
#22115=CARTESIAN_POINT('Ctrl Pts',(18.2670349827885,-0.0605472855394143,
3.29999550882718));
#22116=CARTESIAN_POINT('Ctrl Pts',(18.3147508188514,0.556044050773433,3.57048018084402));
#22117=CARTESIAN_POINT('Ctrl Pts',(18.3624666549143,0.662011579423562,4.23539951180373));
#22118=CARTESIAN_POINT('Ctrl Pts',(18.4101824909771,0.160043688331546,4.684147848987));
#22119=CARTESIAN_POINT('Ctrl Pts',(18.4578983270399,-0.488894784343999,
4.50463268947774));
#22120=CARTESIAN_POINT('Ctrl Pts',(18.5056141631028,-0.68887365394326,3.86170556644909));
#22121=CARTESIAN_POINT('Ctrl Pts',(18.5533299991656,-0.256249247442801,
3.34577634968359));
#22122=CARTESIAN_POINT('Ctrl Pts',(18.6010458352284,0.41169278588589,3.4306307775285));
#22123=CARTESIAN_POINT('Ctrl Pts',(18.6487616712913,0.701570999227752,4.03834572324048));
#22124=CARTESIAN_POINT('Ctrl Pts',(18.6964775073541,0.347185768921481,4.6108472012761));
#22125=CARTESIAN_POINT('Ctrl Pts',(18.744193343417,-0.326025495125306,4.62239829528727));
#22126=CARTESIAN_POINT('Ctrl Pts',(18.7919091794798,-0.699842530451103,
4.06239145790787));
#22127=CARTESIAN_POINT('Ctrl Pts',(18.8396250155426,-0.430983401602837,
3.44508958471478));
#22128=CARTESIAN_POINT('Ctrl Pts',(18.8873408516055,0.233654416470602,3.33737048427408));
#22129=CARTESIAN_POINT('Ctrl Pts',(18.9350566876683,0.683723788661416,3.83815426398688));
#22130=CARTESIAN_POINT('Ctrl Pts',(18.9827725237312,0.505919085286118,4.48756347340344));
#22131=CARTESIAN_POINT('Ctrl Pts',(19.030488359794,-0.136478898681533,4.68923564305365));
#22132=CARTESIAN_POINT('Ctrl Pts',(19.0782041958568,-0.653546209976322,
4.2579721164561));
#22133=CARTESIAN_POINT('Ctrl Pts',(19.1259200319197,-0.570451980578726,
3.58980882586423));
#22134=CARTESIAN_POINT('Ctrl Pts',(19.1736358679825,0.0364970801727598,
3.29833040216201));
#22135=CARTESIAN_POINT('Ctrl Pts',(19.2213517040453,0.609930310515188,3.65120596658116));
#22136=CARTESIAN_POINT('Ctrl Pts',(19.2690675401082,0.623255151928734,4.32438445905389));
#22137=CARTESIAN_POINT('Ctrl Pts',(19.316783376171,0.0642351969327414,4.69967571095415));
#22138=CARTESIAN_POINT('Ctrl Pts',(19.3644992122339,-0.553772927074266,
4.43244399258532));
#22139=CARTESIAN_POINT('Ctrl Pts',(19.4122150482967,-0.663242852612724,
3.76809229994096));
#22140=CARTESIAN_POINT('Ctrl Pts',(19.4599308843595,-0.163646658734412,
3.3167050201661));
#22141=CARTESIAN_POINT('Ctrl Pts',(19.5076467204224,0.486228775054438,3.49279802752061));
#22142=CARTESIAN_POINT('Ctrl Pts',(19.5553625564852,0.689592852244711,4.13466242315333));
#22143=CARTESIAN_POINT('Ctrl Pts',(19.6030783925481,0.259693185238344,4.65286421968052));
#22144=CARTESIAN_POINT('Ctrl Pts',(19.6507942286109,-0.408686697131164,
4.57153080275077));
#22145=CARTESIAN_POINT('Ctrl Pts',(19.6985100646738,-0.701763358503738,
3.96535177039745));
#22146=CARTESIAN_POINT('Ctrl Pts',(19.7462259007365,-0.350399813749482,
3.39099090115443));
#22147=CARTESIAN_POINT('Ctrl Pts',(19.7939417367994,0.322741052541778,3.37589215469092));
#22148=CARTESIAN_POINT('Ctrl Pts',(19.8416575728622,0.699504257835039,3.93392181877779));
#22149=CARTESIAN_POINT('Ctrl Pts',(19.8893734089251,0.433901159015506,4.55263101135276));
#22150=CARTESIAN_POINT('Ctrl Pts',(19.9370892449879,-0.23015857608315,4.663852686053));
#22151=CARTESIAN_POINT('Ctrl Pts',(19.9848050810507,-0.682862933423436,
4.16544436654047));
#22152=CARTESIAN_POINT('Ctrl Pts',(20.0325209171136,-0.508478494849655,
3.51511322409123));
#22153=CARTESIAN_POINT('Ctrl Pts',(20.0802367531764,0.132839643288252,3.31004731418368));
#22154=CARTESIAN_POINT('Ctrl Pts',(20.1279525892393,0.652187835720725,3.73860154375571));
#22155=CARTESIAN_POINT('Ctrl Pts',(20.1756684253021,0.572586513039731,4.4071529569233));
#22156=CARTESIAN_POINT('Ctrl Pts',(20.2233842613649,-0.0327629883405684,
4.70190215105461));
#22157=CARTESIAN_POINT('Ctrl Pts',(20.2711000974278,-0.608151935097038,
4.35190888358257));
#22158=CARTESIAN_POINT('Ctrl Pts',(20.3188159334906,-0.624827148513498,
3.67908301574286));
#22159=CARTESIAN_POINT('Ctrl Pts',(20.3665317695535,-0.0681655280739813,
3.30033184185188));
#22160=CARTESIAN_POINT('Ctrl Pts',(20.4142476056163,0.551956769749184,3.56531418539817));
#22161=CARTESIAN_POINT('Ctrl Pts',(20.4540108023353,0.644905999548395,4.11665253813788));
#22162=CARTESIAN_POINT('Ctrl Pts',(20.4858213597105,0.416382673412033,4.45708139504444));
#22163=CARTESIAN_POINT('Ctrl Pts',(20.509679277742,0.148137151166912,4.60177085628536));
#22164=CARTESIAN_POINT('Ctrl Pts',(20.5335371957734,-0.159214575149101,
4.59858486262053));
#22165=CARTESIAN_POINT('Ctrl Pts',(20.5573951138048,-0.426074836374489,
4.44942877587387));
#22166=CARTESIAN_POINT('Ctrl Pts',(20.5812530318362,-0.589577924844292,
4.19016123618585));
#22167=CARTESIAN_POINT('Ctrl Pts',(20.6051109498677,-0.608473233900696,
3.88450759853215));
#22168=CARTESIAN_POINT('Ctrl Pts',(20.6289688678991,-0.478813304308425,
3.60703485797333));
#22169=CARTESIAN_POINT('Ctrl Pts',(20.6528267859305,-0.231947052182395,
3.42568465323223));
#22170=CARTESIAN_POINT('Ctrl Pts',(20.6766847039619,0.0715712039811096,
3.38475332414555));
#22171=CARTESIAN_POINT('Ctrl Pts',(20.7005426219933,0.357622970648114,3.49427550111266));
#22172=CARTESIAN_POINT('Ctrl Pts',(20.7244005400248,0.556207844932749,3.72745636179159));
#22173=CARTESIAN_POINT('Ctrl Pts',(20.7482584580561,0.618794460414918,4.02728407199912));
#22174=CARTESIAN_POINT('Ctrl Pts',(20.7721163760876,0.530063832205264,4.32043875618714));
#22175=CARTESIAN_POINT('Ctrl Pts',(20.7959742941189,0.311720881859749,4.53523813880796));
#22176=CARTESIAN_POINT('Ctrl Pts',(20.8198322121505,0.01715224242355,4.619156844639));
#22177=CARTESIAN_POINT('Ctrl Pts',(20.8436901301818,-0.281609823618225,
4.55167503361081));
#22178=CARTESIAN_POINT('Ctrl Pts',(20.8675480482133,-0.511511021444125,
4.34929354512778));
#22179=CARTESIAN_POINT('Ctrl Pts',(20.8914059662447,-0.616333626991818,
4.06150032559224));
#22180=CARTESIAN_POINT('Ctrl Pts',(20.9152638842761,-0.570445985619195,
3.75866857192897));
#22181=CARTESIAN_POINT('Ctrl Pts',(20.9391218023075,-0.385068702031786,
3.51484894167474));
#22182=CARTESIAN_POINT('Ctrl Pts',(20.9629797203389,-0.105531663562905,
3.38966195221662));
#22183=CARTESIAN_POINT('Ctrl Pts',(20.9868376383704,0.199810758127152,3.41371924506628));
#22184=CARTESIAN_POINT('Ctrl Pts',(21.0106955564018,0.456293997792742,3.58113815016051));
#22185=CARTESIAN_POINT('Ctrl Pts',(21.0345534744332,0.60120093052663,3.85098018832832));
#22186=CARTESIAN_POINT('Ctrl Pts',(21.0584113924646,0.599097856858477,4.15726162902184));
#22187=CARTESIAN_POINT('Ctrl Pts',(21.082269310496,0.450499039416452,4.42508831804098));
#22188=CARTESIAN_POINT('Ctrl Pts',(21.1061272285275,0.191740934787398,4.58896933394457));
#22189=CARTESIAN_POINT('Ctrl Pts',(21.1299851465589,-0.113903050943465,
4.60883130459215));
#22190=CARTESIAN_POINT('Ctrl Pts',(21.1538430645903,-0.391694638258801,
4.47981743698434));
#22191=CARTESIAN_POINT('Ctrl Pts',(21.1777009826217,-0.573706216867813,
4.23347513609622));
#22192=CARTESIAN_POINT('Ctrl Pts',(21.2015589006531,-0.615430998064313,
3.9300418046833));
#22193=CARTESIAN_POINT('Ctrl Pts',(21.2254168186846,-0.506666136201032,
3.64371515765586));
#22194=CARTESIAN_POINT('Ctrl Pts',(21.2492747367159,-0.27400760274365,3.44450985958179));
#22195=CARTESIAN_POINT('Ctrl Pts',(21.2731326547474,0.0256532534100022,
3.38113703208972));
#22196=CARTESIAN_POINT('Ctrl Pts',(21.2969905727788,0.319041190319967,3.46909305773936));
#22197=CARTESIAN_POINT('Ctrl Pts',(21.3208484908102,0.534414865691478,3.68687029238709));
#22198=CARTESIAN_POINT('Ctrl Pts',(21.3447064088416,0.619109549231529,3.98121627002784));
#22199=CARTESIAN_POINT('Ctrl Pts',(21.3685643268731,0.552415083779586,4.28015538130547));
#22200=CARTESIAN_POINT('Ctrl Pts',(21.3924222449044,0.350640082858436,4.51058887057447));
#22201=CARTESIAN_POINT('Ctrl Pts',(21.4162801629359,0.0631240304344945,
4.61616947282646));
#22202=CARTESIAN_POINT('Ctrl Pts',(21.4401380809673,-0.239827566894842,
4.57107985485291));
#22203=CARTESIAN_POINT('Ctrl Pts',(21.4639959989987,-0.484134791346583,
4.38634565646493));
#22204=CARTESIAN_POINT('Ctrl Pts',(21.4878539170302,-0.610057871747176,
4.10713942122688));
#22205=CARTESIAN_POINT('Ctrl Pts',(21.5117118350615,-0.586805184862796,
3.80173467907963));
#22206=CARTESIAN_POINT('Ctrl Pts',(21.535569753093,-0.420062646027161,3.5448112085363));
#22207=CARTESIAN_POINT('Ctrl Pts',(21.5594276711244,-0.150603347961132,
3.39919379659958));
#22208=CARTESIAN_POINT('Ctrl Pts',(21.5832855891558,0.155682571034224,3.40048986702667));
#22209=CARTESIAN_POINT('Ctrl Pts',(21.6071435071872,0.423899860703612,3.54838249529388));
#22210=CARTESIAN_POINT('Ctrl Pts',(21.6310014252187,0.588462087630599,3.80670790527556));
#22211=CARTESIAN_POINT('Ctrl Pts',(21.6548593432501,0.609129304746478,4.11229849758833));
#22212=CARTESIAN_POINT('Ctrl Pts',(21.6787172612815,0.480847814502724,4.39042904829107));
#22213=CARTESIAN_POINT('Ctrl Pts',(21.7025751793129,0.234985935581564,4.57308906161293));
#22214=CARTESIAN_POINT('Ctrl Pts',(21.7264330973443,-0.0683364054776661,
4.61561318873779));
#22215=CARTESIAN_POINT('Ctrl Pts',(21.7502910153758,-0.35494863395129,4.5076031222497));
#22216=CARTESIAN_POINT('Ctrl Pts',(21.7741489334072,-0.554766252817153,
4.2754702655401));
#22217=CARTESIAN_POINT('Ctrl Pts',(21.7980068514386,-0.618928411339905,
3.9759774252466));
#22218=CARTESIAN_POINT('Ctrl Pts',(21.82186476947,-0.531745714018629,3.68235875884208));
#22219=CARTESIAN_POINT('Ctrl Pts',(21.8457226875014,-0.314536705157368,
3.46641202827438));
#22220=CARTESIAN_POINT('Ctrl Pts',(21.8695806055329,-0.0204149040773093,
3.3809420914381));
#22221=CARTESIAN_POINT('Ctrl Pts',(21.8934385235643,0.278698897140474,3.44684867604406));
#22222=CARTESIAN_POINT('Ctrl Pts',(21.9172964415957,0.509663226401888,3.6480158268968));
#22223=CARTESIAN_POINT('Ctrl Pts',(21.9411543596271,0.616001013860485,3.93525269592965));
#22224=CARTESIAN_POINT('Ctrl Pts',(21.9650122776585,0.571709773899469,4.23832204448885));
#22225=CARTESIAN_POINT('Ctrl Pts',(21.98887019569,0.387619921158457,4.48311516140836));
#22226=CARTESIAN_POINT('Ctrl Pts',(22.0127281137213,0.108746439139576,4.60977346157076));
#22227=CARTESIAN_POINT('Ctrl Pts',(22.0365860317528,-0.196718509442517,
4.5873255404835));
#22228=CARTESIAN_POINT('Ctrl Pts',(22.0604439497842,-0.454080423961193,
4.42126052632156));
#22229=CARTESIAN_POINT('Ctrl Pts',(22.0843018678156,-0.600407305919173,
4.15218583856754));
#22230=CARTESIAN_POINT('Ctrl Pts',(22.1081597858471,-0.599918246812857,
3.84589756782496));
#22231=CARTESIAN_POINT('Ctrl Pts',(22.1320177038785,-0.452732834916613,
3.57729153941473));
#22232=CARTESIAN_POINT('Ctrl Pts',(22.1558756219099,-0.194841912687001,
3.41204924396571));
#22233=CARTESIAN_POINT('Ctrl Pts',(22.1797335399413,0.110693164578993,3.39057692382254));
#22234=CARTESIAN_POINT('Ctrl Pts',(22.2035914579728,0.389160747889314,3.51812514615901));
#22235=CARTESIAN_POINT('Ctrl Pts',(22.2274493760041,0.572467927805029,3.76350489626149));
#22236=CARTESIAN_POINT('Ctrl Pts',(22.2513072940356,0.615791105677536,4.06671414123586));
#22237=CARTESIAN_POINT('Ctrl Pts',(22.2751652120669,0.508536584364246,4.35360996140145));
#22238=CARTESIAN_POINT('Ctrl Pts',(22.2990231300984,0.276931015980992,4.55403851389998));
#22239=CARTESIAN_POINT('Ctrl Pts',(22.3228810481298,-0.0223917293827815,
4.61898955797298));
#22240=CARTESIAN_POINT('Ctrl Pts',(22.3467389661613,-0.31623908674035,4.53258079431836));
#22241=CARTESIAN_POINT('Ctrl Pts',(22.3705968841927,-0.532757373651304,
4.31594151899069));
#22242=CARTESIAN_POINT('Ctrl Pts',(22.3944548022241,-0.619001969851995,
4.02204593667267));
#22243=CARTESIAN_POINT('Ctrl Pts',(22.4183127202555,-0.553883724721699,
3.72275952141814));
#22244=CARTESIAN_POINT('Ctrl Pts',(22.4421706382869,-0.35332581843718,3.49126595675675));
#22245=CARTESIAN_POINT('Ctrl Pts',(22.4660285563184,-0.0663701307507445,
3.38417172009386));
#22246=CARTESIAN_POINT('Ctrl Pts',(22.4898864743497,0.236814872379406,3.42766427875767));
#22247=CARTESIAN_POINT('Ctrl Pts',(22.5137443923812,0.482092168510832,3.61110849992699));
#22248=CARTESIAN_POINT('Ctrl Pts',(22.5376023104126,0.609484835267769,3.88964730767638));
#22249=CARTESIAN_POINT('Ctrl Pts',(22.561460228444,0.587841786482003,4.19517031382209));
#22250=CARTESIAN_POINT('Ctrl Pts',(22.5853181464754,0.422455543015367,4.45296893898932));
#22251=CARTESIAN_POINT('Ctrl Pts',(22.6091760645069,0.153767157666155,4.60000417439789));
#22252=CARTESIAN_POINT('Ctrl Pts',(22.6330339825383,-0.152521006364708,
4.60032232020799));
#22253=CARTESIAN_POINT('Ctrl Pts',(22.6568919005697,-0.421514535902825,
4.45384478734481));
#22254=CARTESIAN_POINT('Ctrl Pts',(22.6807498186011,-0.587434568575047,
4.19639082134502));
#22255=CARTESIAN_POINT('Ctrl Pts',(22.7046077366325,-0.60971407867596,3.89091209973551));
#22256=CARTESIAN_POINT('Ctrl Pts',(22.728465654664,-0.482895786937606,3.61211183522625));
#22257=CARTESIAN_POINT('Ctrl Pts',(22.7523235726954,-0.23800784887647,3.4281541921173));
#22258=CARTESIAN_POINT('Ctrl Pts',(22.7761814907268,0.0651013135850054,
3.38404091701771));
#22259=CARTESIAN_POINT('Ctrl Pts',(22.8000394087582,0.352249768808992,3.49052260401466));
#22260=CARTESIAN_POINT('Ctrl Pts',(22.8238973267896,0.553345940411564,3.72163220123786));
#22261=CARTESIAN_POINT('Ctrl Pts',(22.8398026054772,0.597082876783669,3.92101540361374));
#22262=CARTESIAN_POINT('Ctrl Pts',(22.847755244821,0.593766187829899,4.01991291515446));
#22263=CARTESIAN_POINT('',(22.8,0.337479661717902,3.51106003648017));
#22264=CARTESIAN_POINT('Ctrl Pts',(22.8,0.337504360408405,3.51101527402275));
#22265=CARTESIAN_POINT('Ctrl Pts',(22.8,0.337610992569967,3.51114843896934));
#22266=CARTESIAN_POINT('Ctrl Pts',(22.8,0.337717562131928,3.51128164981369));
#22267=CARTESIAN_POINT('Ctrl Pts',(22.8,0.337824069051012,3.51141490653789));
#22268=CARTESIAN_POINT('Ctrl Pts',(22.8,0.354145371784291,3.53183539523119));
#22269=CARTESIAN_POINT('Ctrl Pts',(22.8,0.368999739942303,3.55333386321799));
#22270=CARTESIAN_POINT('Ctrl Pts',(22.8,0.382262544471458,3.57576050230915));
#22271=CARTESIAN_POINT('Ctrl Pts',(22.8,0.395177725624396,3.59759933027929));
#22272=CARTESIAN_POINT('Ctrl Pts',(22.8,0.406583379369087,3.62031953557487));
#22273=CARTESIAN_POINT('Ctrl Pts',(22.8,0.416319965152677,3.64376476659274));
#22274=CARTESIAN_POINT('Ctrl Pts',(22.8,0.420499854003763,3.65382973822867));
#22275=CARTESIAN_POINT('Ctrl Pts',(22.8,0.424371599987778,3.66402799385056));
#22276=CARTESIAN_POINT('Ctrl Pts',(22.8,0.42792023461967,3.67434527679585));
#22277=CARTESIAN_POINT('Ctrl Pts',(22.8,0.430015882150509,3.68043815216119));
#22278=CARTESIAN_POINT('Ctrl Pts',(22.8,0.431995626466768,3.68656321156818));
#22279=CARTESIAN_POINT('Ctrl Pts',(22.8,0.433857425300493,3.69271766785326));
#22280=CARTESIAN_POINT('Ctrl Pts',(22.8,0.440667704273582,3.71523007009016));
#22281=CARTESIAN_POINT('Ctrl Pts',(22.8,0.445903532435623,3.73813926926309));
#22282=CARTESIAN_POINT('Ctrl Pts',(22.8,0.449441836754149,3.76130640751661));
#22283=CARTESIAN_POINT('Ctrl Pts',(22.8,0.450038513826676,3.76521316594877));
#22284=CARTESIAN_POINT('Ctrl Pts',(22.8,0.450586822418701,3.76912718643627));
#22285=CARTESIAN_POINT('Ctrl Pts',(22.8,0.451086059471329,3.77304770583064));
#22286=CARTESIAN_POINT('Ctrl Pts',(22.8,0.453684096906641,3.79345015011803));
#22287=CARTESIAN_POINT('Ctrl Pts',(22.8,0.454954433743694,3.81403106227893));
#22288=CARTESIAN_POINT('Ctrl Pts',(22.8,0.45484641916779,3.83463783350426));
#22289=CARTESIAN_POINT('Ctrl Pts',(22.8,0.454808390965019,3.84189276616533));
#22290=CARTESIAN_POINT('Ctrl Pts',(22.8,0.454599381710613,3.84915061719132));
#22291=CARTESIAN_POINT('Ctrl Pts',(22.8,0.454216814112443,3.8564037154462));
#22292=CARTESIAN_POINT('Ctrl Pts',(22.8,0.453866695925276,3.86304160538904));
#22293=CARTESIAN_POINT('Ctrl Pts',(22.8,0.453371644107099,3.86966645154658));
#22294=CARTESIAN_POINT('Ctrl Pts',(22.8,0.452731182295137,3.87626933737115));
#22295=CARTESIAN_POINT('Ctrl Pts',(22.8,0.450713457978438,3.89707120727158));
#22296=CARTESIAN_POINT('Ctrl Pts',(22.8,0.447253508643,3.9176725514372));
#22297=CARTESIAN_POINT('Ctrl Pts',(22.8,0.442312061254715,3.9379035771693));
#22298=CARTESIAN_POINT('Ctrl Pts',(22.8,0.437564183511961,3.95734209977996));
#22299=CARTESIAN_POINT('Ctrl Pts',(22.8,0.431447509288203,3.97643919003209));
#22300=CARTESIAN_POINT('Ctrl Pts',(22.8,0.423915075143768,3.9949978423605));
#22301=CARTESIAN_POINT('Ctrl Pts',(22.8,0.421325190817866,4.00137888225459));
#22302=CARTESIAN_POINT('Ctrl Pts',(22.8,0.418567902041021,4.00769582483512));
#22303=CARTESIAN_POINT('Ctrl Pts',(22.8,0.415641328671541,4.01393920819689));
#22304=CARTESIAN_POINT('Ctrl Pts',(22.6211545887425,-1.51173456864708E-7,
4.59404872180247));
#22305=CARTESIAN_POINT('Ctrl Pts',(22.6251143866744,-0.0492822808754852,
4.59404929162283));
#22306=CARTESIAN_POINT('Ctrl Pts',(22.6290741846063,-0.0985642856931001,
4.58798571459226));
#22307=CARTESIAN_POINT('Ctrl Pts',(22.6330339825383,-0.14630523394925,4.57585637376244));
#22308=CARTESIAN_POINT('Ctrl Pts',(22.6409866218821,-0.242185516210759,
4.55149647592026));
#22309=CARTESIAN_POINT('Ctrl Pts',(22.6489392612259,-0.331850026056775,
4.50267063163255));
#22310=CARTESIAN_POINT('Ctrl Pts',(22.6568919005697,-0.404335619758509,
4.43534871515538));
#22311=CARTESIAN_POINT('Ctrl Pts',(22.6648445399135,-0.476821213460227,
4.36802679867822));
#22312=CARTESIAN_POINT('Ctrl Pts',(22.6727971792573,-0.532127891017642,
4.28220881001161));
#22313=CARTESIAN_POINT('Ctrl Pts',(22.6807498186011,-0.563494481479829,
4.18838669541007));
#22314=CARTESIAN_POINT('Ctrl Pts',(22.6887024579449,-0.594861071942019,
4.09456458080851));
#22315=CARTESIAN_POINT('Ctrl Pts',(22.6966550972887,-0.602287575308989,
3.99273834027202));
#22316=CARTESIAN_POINT('Ctrl Pts',(22.7046077366325,-0.584864445036083,
3.89535850925222));
#22317=CARTESIAN_POINT('Ctrl Pts',(22.7125603759763,-0.567441314763176,
3.79797867823242));
#22318=CARTESIAN_POINT('Ctrl Pts',(22.7205130153201,-0.525168550850394,
3.70504525672934));
#22319=CARTESIAN_POINT('Ctrl Pts',(22.7284656546639,-0.463217512550482,
3.62791893879298));
#22320=CARTESIAN_POINT('Ctrl Pts',(22.7364182940078,-0.401266474250563,
3.5507926208566));
#22321=CARTESIAN_POINT('Ctrl Pts',(22.7443709333516,-0.319637161563486,
3.48947340648693));
#22322=CARTESIAN_POINT('Ctrl Pts',(22.7523235726954,-0.228304311476372,
3.45146158678551));
#22323=CARTESIAN_POINT('Ctrl Pts',(22.7602762120392,-0.136971461389268,
3.41344976708409));
#22324=CARTESIAN_POINT('Ctrl Pts',(22.768228851383,-0.0359350739021178,
3.3987453420509));
#22325=CARTESIAN_POINT('Ctrl Pts',(22.7761814907268,0.062441195712126,3.40914007736714));
#22326=CARTESIAN_POINT('Ctrl Pts',(22.7841209938178,0.160654966376612,3.41951764255099));
#22327=CARTESIAN_POINT('Ctrl Pts',(22.7920604969089,0.256217399931083,3.45491151845628));
#22328=CARTESIAN_POINT('Ctrl Pts',(22.8,0.337504360408238,3.51101527402264));
#22329=CARTESIAN_POINT('',(4.,-0.219892372742957,4.3529863453938));
#22330=CARTESIAN_POINT('Ctrl Pts',(4.,-0.219914231356238,4.35301468169996));
#22331=CARTESIAN_POINT('Ctrl Pts',(4.,-0.219843051329574,4.3531167999744));
#22332=CARTESIAN_POINT('Ctrl Pts',(4.,-0.219771822781512,4.35321888245988));
#22333=CARTESIAN_POINT('Ctrl Pts',(4.,-0.21970054575756,4.3533209291203));
#22334=CARTESIAN_POINT('Ctrl Pts',(4.,-0.207925336055227,4.3701793886806));
#22335=CARTESIAN_POINT('Ctrl Pts',(4.,-0.194831304039315,4.38605734350833));
#22336=CARTESIAN_POINT('Ctrl Pts',(4.,-0.18064579384139,4.40088380688851));
#22337=CARTESIAN_POINT('Ctrl Pts',(4.,-0.168975273508986,4.41308164397169));
#22338=CARTESIAN_POINT('Ctrl Pts',(4.,-0.156565051628872,4.42456888924957));
#22339=CARTESIAN_POINT('Ctrl Pts',(4.,-0.143515931303371,4.43531683418355));
#22340=CARTESIAN_POINT('Ctrl Pts',(4.,-0.133182439541062,4.44382804395605));
#22341=CARTESIAN_POINT('Ctrl Pts',(4.,-0.122447811630206,4.45187590303098));
#22342=CARTESIAN_POINT('Ctrl Pts',(4.,-0.111352162047151,4.45944712768208));
#22343=CARTESIAN_POINT('Ctrl Pts',(4.,-0.105068105051177,4.46373511522897));
#22344=CARTESIAN_POINT('Ctrl Pts',(4.,-0.0986661212125077,4.46787107983396));
#22345=CARTESIAN_POINT('Ctrl Pts',(4.,-0.0921733602714696,4.47184061613108));
#22346=CARTESIAN_POINT('Ctrl Pts',(4.,-0.0718171345235072,4.48428598070136));
#22347=CARTESIAN_POINT('Ctrl Pts',(4.,-0.0505350523745213,4.49512244469223));
#22348=CARTESIAN_POINT('Ctrl Pts',(4.,-0.0285775088988711,4.50429938857761));
#22349=CARTESIAN_POINT('Ctrl Pts',(4.,-0.00645956782426854,4.51354336909515));
#22350=CARTESIAN_POINT('Ctrl Pts',(4.,0.0163444141029789,4.52110543571878));
#22351=CARTESIAN_POINT('Ctrl Pts',(4.,0.0396343143342583,4.52702898180467));
#22352=CARTESIAN_POINT('Ctrl Pts',(4.,0.0479455316904685,4.52914285427945));
#22353=CARTESIAN_POINT('Ctrl Pts',(4.,0.0563191235587283,4.53104786585874));
#22354=CARTESIAN_POINT('Ctrl Pts',(4.,0.0647475081636451,4.53274519105122));
#22355=CARTESIAN_POINT('Ctrl Pts',(4.,0.0709442475001029,4.53399310299165));
#22356=CARTESIAN_POINT('Ctrl Pts',(4.,0.0771669940275102,4.53512789739638));
#22357=CARTESIAN_POINT('Ctrl Pts',(4.,0.0834037601527001,4.53614909266968));
#22358=CARTESIAN_POINT('Ctrl Pts',(4.,0.108500755516298,4.54025842313435));
#22359=CARTESIAN_POINT('Ctrl Pts',(4.,0.133859781029961,4.54253781872753));
#22360=CARTESIAN_POINT('Ctrl Pts',(3.99999999999999,0.159256593756596,4.54305292380224));
#22361=CARTESIAN_POINT('Ctrl Pts',(3.99999999999999,0.185497795908202,4.5435851550133));
#22362=CARTESIAN_POINT('Ctrl Pts',(3.99999999999998,0.211780221987087,4.54223483664603));
#22363=CARTESIAN_POINT('Ctrl Pts',(3.99999999999998,0.237902321580844,4.5390442708621));
#22364=CARTESIAN_POINT('Ctrl Pts',(3.99999999999998,0.243507595489062,4.53835964001621));
#22365=CARTESIAN_POINT('Ctrl Pts',(3.99999999999998,0.249105619801251,4.53759013757336));
#22366=CARTESIAN_POINT('Ctrl Pts',(3.99999999999998,0.254694598474614,4.53673594206822));
#22367=CARTESIAN_POINT('Ctrl Pts',(4.,-0.219914231356244,4.35301468169996));
#22368=CARTESIAN_POINT('Ctrl Pts',(4.00793950309107,-0.278596966840389,
4.31645650682028));
#22369=CARTESIAN_POINT('Ctrl Pts',(4.02383164552594,-0.377405665439666,
4.21337674819164));
#22370=CARTESIAN_POINT('Ctrl Pts',(4.04767642730463,-0.433534992178268,
4.00656196868444));
#22371=CARTESIAN_POINT('Ctrl Pts',(4.07153434533603,-0.383670022685343,
3.79803920418254));
#22372=CARTESIAN_POINT('Ctrl Pts',(4.09539226336747,-0.239994733226421,
3.63889579340969));
#22373=CARTESIAN_POINT('Ctrl Pts',(4.11925018139887,-0.0376302499649443,
3.56805514133307));
#22374=CARTESIAN_POINT('Ctrl Pts',(4.1431080994303,0.173933765839147,3.60283521426327));
#22375=CARTESIAN_POINT('Ctrl Pts',(4.16696601746172,0.342967344134064,3.73473372141871));
#22376=CARTESIAN_POINT('Ctrl Pts',(4.19082393549313,0.428135478754777,3.93149662217858));
#22377=CARTESIAN_POINT('Ctrl Pts',(4.21468185352456,0.40861313688017,4.1450106963618));
#22378=CARTESIAN_POINT('Ctrl Pts',(4.23853977155597,0.289173588337559,4.32306558264197));
#22379=CARTESIAN_POINT('Ctrl Pts',(4.25811226835493,0.13317859508208,4.40432939198872));
#22380=CARTESIAN_POINT('Ctrl Pts',(4.26973212581007,0.0319512750557707,
4.41584666103033));
#22381=CARTESIAN_POINT('Ctrl Pts',(4.2733993439214,2.51014653359152E-6,
4.41583996132385));
#22382=CARTESIAN_POINT('Origin',(3.42660065607856,0.,4.));
#22383=CARTESIAN_POINT('',(4.,-0.219892372743086,3.64701365460628));
#22384=CARTESIAN_POINT('Origin',(4.,0.,4.));
#22385=CARTESIAN_POINT('Ctrl Pts',(4.,-0.219892372743211,3.64701365460636));
#22386=CARTESIAN_POINT('Ctrl Pts',(4.00795263934381,-0.161099076858729,
3.61038844940468));
#22387=CARTESIAN_POINT('Ctrl Pts',(4.02385791803142,-0.0249198690254346,
3.56711791692558));
#22388=CARTESIAN_POINT('Ctrl Pts',(4.04771583606284,0.185569069288609,3.60813812632505));
#22389=CARTESIAN_POINT('Ctrl Pts',(4.07157375409426,0.350624105231944,3.74494568050885));
#22390=CARTESIAN_POINT('Ctrl Pts',(4.09543167212568,0.429971014252744,3.94413788601839));
#22391=CARTESIAN_POINT('Ctrl Pts',(4.1192895901571,0.40416308778273,4.15698104289539));
#22392=CARTESIAN_POINT('Ctrl Pts',(4.14314750818851,0.279534313346206,4.3314427366163));
#22393=CARTESIAN_POINT('Ctrl Pts',(4.16225119682902,0.125004509401131,4.40624063703925));
#22394=CARTESIAN_POINT('Ctrl Pts',(4.1734022461257,0.0278694809177792,4.41585864517498));
#22395=CARTESIAN_POINT('Ctrl Pts',(4.17660065607858,5.88453344126799E-6,
4.41584444980552));
#22396=CARTESIAN_POINT('Ctrl Pts',(3.95224475517896,-0.314128184302177,
3.49573985500833));
#22397=CARTESIAN_POINT('Ctrl Pts',(3.96019739452277,-0.230138771413741,
3.44341876234755));
#22398=CARTESIAN_POINT('Ctrl Pts',(3.97610267321038,-0.0355993848822847,
3.38160445914153));
#22399=CARTESIAN_POINT('Ctrl Pts',(3.9999605912418,0.265095483172694,3.44020405374152));
#22400=CARTESIAN_POINT('Ctrl Pts',(4.02381850927322,0.500885556761892,3.63564106712445));
#22401=CARTESIAN_POINT('Ctrl Pts',(4.04767642730465,0.614236921112272,3.92019793948569));
#22402=CARTESIAN_POINT('Ctrl Pts',(4.07153434533605,0.577368897990231,4.22425593648149));
#22403=CARTESIAN_POINT('Ctrl Pts',(4.09539226336749,0.399329932212592,4.47348393104611));
#22404=CARTESIAN_POINT('Ctrl Pts',(4.11925018139889,0.123637843932736,4.60692867011962));
#22405=CARTESIAN_POINT('Ctrl Pts',(4.14310809943032,-0.182283847264271,
4.59196468982869));
#22406=CARTESIAN_POINT('Ctrl Pts',(4.16696601746173,-0.443633876576525,
4.43224822622665));
#22407=CARTESIAN_POINT('Ctrl Pts',(4.19082393549315,-0.596502436238336,
4.16683582239239));
#22408=CARTESIAN_POINT('Ctrl Pts',(4.21468185352458,-0.603510379797736,
3.86062723727387));
#22409=CARTESIAN_POINT('Ctrl Pts',(4.23853977155598,-0.462943343075553,
3.58849923641164));
#22410=CARTESIAN_POINT('Ctrl Pts',(4.26239768958742,-0.209174182705692,
3.41699430327496));
#22411=CARTESIAN_POINT('Ctrl Pts',(4.28625560761882,0.0957438341235747,
3.38805018506757));
#22412=CARTESIAN_POINT('Ctrl Pts',(4.31011352565025,0.377249837899377,3.50874444390425));
#22413=CARTESIAN_POINT('Ctrl Pts',(4.33397144368167,0.566508000142931,3.7495640793295));
#22414=CARTESIAN_POINT('Ctrl Pts',(4.35782936171309,0.617239514437223,4.05162211295782));
#22415=CARTESIAN_POINT('Ctrl Pts',(4.3816872797445,0.517039159770137,4.34105713706075));
#22416=CARTESIAN_POINT('Ctrl Pts',(4.40554519777592,0.290408643717306,4.54709439922074));
#22417=CARTESIAN_POINT('Ctrl Pts',(4.42940311580735,-0.00723469473045889,
4.61935217913086));
#22418=CARTESIAN_POINT('Ctrl Pts',(4.45326103383876,-0.303108954077165,
4.54016147994594));
#22419=CARTESIAN_POINT('Ctrl Pts',(4.47711895187019,-0.524864817190473,
4.3288865854667));
#22420=CARTESIAN_POINT('Ctrl Pts',(4.5009768699016,-0.618276935702851,4.03718996201469));
#22421=CARTESIAN_POINT('Ctrl Pts',(4.52483478793302,-0.560503501787052,
3.7363993798876));
#22422=CARTESIAN_POINT('Ctrl Pts',(4.54869270596444,-0.365671693940747,
3.50006632967672));
#22423=CARTESIAN_POINT('Ctrl Pts',(4.57255062399586,-0.0814231961944085,
3.38598067979976));
#22424=CARTESIAN_POINT('Ctrl Pts',(4.59640854202727,0.222735490926488,3.42203947925158));
#22425=CARTESIAN_POINT('Ctrl Pts',(4.6202664600587,0.472429283332598,3.59942536936051));
#22426=CARTESIAN_POINT('Ctrl Pts',(4.64412437809011,0.606601247243452,3.87476266809168));
#22427=CARTESIAN_POINT('Ctrl Pts',(4.66798229612153,0.592442682719785,4.18072390587243));
#22428=CARTESIAN_POINT('Ctrl Pts',(4.69184021415295,0.433415744455024,4.44249322584619));
#22429=CARTESIAN_POINT('Ctrl Pts',(4.71569813218437,0.168406850663934,4.59606089882753));
#22430=CARTESIAN_POINT('Ctrl Pts',(4.7395560502158,-0.1377821054254,4.60387544567241));
#22431=CARTESIAN_POINT('Ctrl Pts',(4.7634139682472,-0.410279583628813,4.46402599681362));
#22432=CARTESIAN_POINT('Ctrl Pts',(4.78727188627863,-0.582452527843622,
4.21070955191949));
#22433=CARTESIAN_POINT('Ctrl Pts',(4.81112980431005,-0.612199963312297,
3.9058688819681));
#22434=CARTESIAN_POINT('Ctrl Pts',(4.83498772234147,-0.492247831758966,
3.62404583445569));
#22435=CARTESIAN_POINT('Ctrl Pts',(4.85884564037289,-0.251927696778831,
3.4341538212047));
#22436=CARTESIAN_POINT('Ctrl Pts',(4.88270355840431,0.0499956224363984,
3.38262661200963));
#22437=CARTESIAN_POINT('Ctrl Pts',(4.90656147643572,0.339693650112522,3.48206401309162));
#22438=CARTESIAN_POINT('Ctrl Pts',(4.93041939446714,0.546327327266884,3.70815087126575));
#22439=CARTESIAN_POINT('Ctrl Pts',(4.95427731249857,0.619369091246891,4.00560279122603));
#22440=CARTESIAN_POINT('Ctrl Pts',(4.97813523052998,0.540958241141728,4.3016846761146));
#22441=CARTESIAN_POINT('Ctrl Pts',(5.00199314856141,0.330268365670778,4.52399643996756));
#22442=CARTESIAN_POINT('Ctrl Pts',(5.02585106659282,0.0388188784636707,
4.61817680087201));
#22443=CARTESIAN_POINT('Ctrl Pts',(5.04970898462424,-0.262122881932824,
4.56119609516527));
#22444=CARTESIAN_POINT('Ctrl Pts',(5.07356690265566,-0.498968457612796,
4.36698765751594));
#22445=CARTESIAN_POINT('Ctrl Pts',(5.09742482068708,-0.613802653778546,
4.08304074106085));
#22446=CARTESIAN_POINT('Ctrl Pts',(5.12128273871849,-0.578545381446849,
3.77878810143205));
#22447=CARTESIAN_POINT('Ctrl Pts',(5.14514065674992,-0.40181800409162,3.52862779669421));
#22448=CARTESIAN_POINT('Ctrl Pts',(5.16899857478133,-0.126835179433317,
3.39373083558568));
#22449=CARTESIAN_POINT('Ctrl Pts',(5.19285649281276,0.179162301517353,3.4070831996169));
#22450=CARTESIAN_POINT('Ctrl Pts',(5.21671441084417,0.441349719463922,3.56541987207117));
#22451=CARTESIAN_POINT('Ctrl Pts',(5.24057232887559,0.595615108876583,3.83002322352904));
#22452=CARTESIAN_POINT('Ctrl Pts',(5.26443024690701,0.604236379939102,4.13619052690848));
#22453=CARTESIAN_POINT('Ctrl Pts',(5.28828816493843,0.465105397037983,4.40905553670335));
#22454=CARTESIAN_POINT('Ctrl Pts',(5.31214608296985,0.21224347534444,4.58189532532512));
#22455=CARTESIAN_POINT('Ctrl Pts',(5.33600400100126,-0.0925177574670201,
4.61244585639451));
#22456=CARTESIAN_POINT('Ctrl Pts',(5.35986191903269,-0.37465587844466,4.49323669288525));
#22457=CARTESIAN_POINT('Ctrl Pts',(5.3837198370641,-0.565180431721392,4.25341772246777));
#22458=CARTESIAN_POINT('Ctrl Pts',(5.40757775509553,-0.617502974236318,
3.95163121594683));
#22459=CARTESIAN_POINT('Ctrl Pts',(5.43143567312694,-0.518829219107294,
3.66167219466597));
#22460=CARTESIAN_POINT('Ctrl Pts',(5.45529359115837,-0.293287587282116,
3.45444353765392));
#22461=CARTESIAN_POINT('Ctrl Pts',(5.47915150918978,0.00397084862654925,
3.38061829634467));
#22462=CARTESIAN_POINT('Ctrl Pts',(5.50300942722121,0.300258303883157,3.45824875319892));
#22463=CARTESIAN_POINT('Ctrl Pts',(5.52686734525262,0.523124424966688,3.66835214690199));
#22464=CARTESIAN_POINT('Ctrl Pts',(5.55072526328404,0.618072374525773,3.95955247459688));
#22465=CARTESIAN_POINT('Ctrl Pts',(5.57458318131546,0.561884792553919,4.26064332401524));
#22466=CARTESIAN_POINT('Ctrl Pts',(5.59844109934688,0.368301073379394,4.49799978094171));
#22467=CARTESIAN_POINT('Ctrl Pts',(5.62229901737829,0.0846577094226282,
4.61358172616469));
#22468=CARTESIAN_POINT('Ctrl Pts',(5.64615693540972,-0.219686770477705,
4.57912622575047));
#22469=CARTESIAN_POINT('Ctrl Pts',(5.67001485344113,-0.470311850924231,
4.40305858798173));
#22470=CARTESIAN_POINT('Ctrl Pts',(5.69387277147256,-0.605932872639677,
4.12843214650112));
#22471=CARTESIAN_POINT('Ctrl Pts',(5.71773068950397,-0.593386801983745,
3.82240054650545));
#22472=CARTESIAN_POINT('Ctrl Pts',(5.74158860753539,-0.435741494202748,
3.55979685111874));
#22473=CARTESIAN_POINT('Ctrl Pts',(5.76544652556682,-0.171545522688555,
3.40483481554927));
#22474=CARTESIAN_POINT('Ctrl Pts',(5.78930444359822,0.134598003740687,3.39540688139736));
#22475=CARTESIAN_POINT('Ctrl Pts',(5.81316236162965,0.407828648458881,3.53381843004554));
#22476=CARTESIAN_POINT('Ctrl Pts',(5.83702027966106,0.58133408605803,3.78622407765735));
#22477=CARTESIAN_POINT('Ctrl Pts',(5.86087819769249,0.612687492198482,4.09090374899912));
#22478=CARTESIAN_POINT('Ctrl Pts',(5.8847361157239,0.494222140250734,4.3733550009975));
#22479=CARTESIAN_POINT('Ctrl Pts',(5.90859403375532,0.254905969192102,4.56451074097759));
#22480=CARTESIAN_POINT('Ctrl Pts',(5.93245195178675,-0.0467415727364197,
4.61762831145024));
#22481=CARTESIAN_POINT('Ctrl Pts',(5.95630986981815,-0.336959681931401,
4.51971877801409));
#22482=CARTESIAN_POINT('Ctrl Pts',(5.98016778784959,-0.544781677596122,
4.29472414464893));
#22483=CARTESIAN_POINT('Ctrl Pts',(6.00402570588099,-0.61939026621187,3.99766086682344));
#22484=CARTESIAN_POINT('Ctrl Pts',(6.02788362391242,-0.542540019317823,
3.70117063377655));
#22485=CARTESIAN_POINT('Ctrl Pts',(6.05174154194384,-0.333025929677459,
3.47775031355921));
#22486=CARTESIAN_POINT('Ctrl Pts',(6.07559945997526,-0.042074208138152,
3.38203805739984));
#22487=CARTESIAN_POINT('Ctrl Pts',(6.09945737800668,0.259158778028439,3.43742717299816));
#22488=CARTESIAN_POINT('Ctrl Pts',(6.12331529603809,0.497033648893269,3.63039418124561));
#22489=CARTESIAN_POINT('Ctrl Pts',(6.14717321406952,0.613345206175343,3.91371436613889));
#22490=CARTESIAN_POINT('Ctrl Pts',(6.17103113210093,0.579724447951105,4.21818191418763));
#22491=CARTESIAN_POINT('Ctrl Pts',(6.19488905013236,0.40425597056565,4.46920707734689));
#22492=CARTESIAN_POINT('Ctrl Pts',(6.21874696816377,0.13010450107023,4.60567007851858));
#22493=CARTESIAN_POINT('Ctrl Pts',(6.24260488619519,-0.176179318911185,
4.59370602015056));
#22494=CARTESIAN_POINT('Ctrl Pts',(6.26646280422661,-0.438782409775579,
4.43717629804221));
#22495=CARTESIAN_POINT('Ctrl Pts',(6.29032072225803,-0.595217424383659,
4.17259489198797));
#22496=CARTESIAN_POINT('Ctrl Pts',(6.31417864028945,-0.604035436411749,
3.86794272465182));
#22497=CARTESIAN_POINT('Ctrl Pts',(6.34598919766468,-0.423477061217623,
3.4998212904071));
#22498=CARTESIAN_POINT('Ctrl Pts',(6.3857523943837,0.100470573235224,3.30464850830547));
#22499=CARTESIAN_POINT('Ctrl Pts',(6.43346823044655,0.640013163212275,3.70919899990029));
#22500=CARTESIAN_POINT('Ctrl Pts',(6.48118406650937,0.590335835129396,4.3806576914582));
#22501=CARTESIAN_POINT('Ctrl Pts',(6.52889990257223,-0.000686065451295705,
4.70262946694599));
#22502=CARTESIAN_POINT('Ctrl Pts',(6.57661573863505,-0.591483599613884,
4.37932465573422));
#22503=CARTESIAN_POINT('Ctrl Pts',(6.6243315746979,-0.638898060441451,3.70770201230499));
#22504=CARTESIAN_POINT('Ctrl Pts',(6.67204741076074,-0.0997162142428727,
3.30448953810453));
#22505=CARTESIAN_POINT('Ctrl Pts',(6.71976324682356,0.531096731682035,3.53998115137447));
#22506=CARTESIAN_POINT('Ctrl Pts',(6.76747908288643,0.674163513320998,4.19791190586338));
#22507=CARTESIAN_POINT('Ctrl Pts',(6.81519491894923,0.19815244237474,4.67409883091767));
#22508=CARTESIAN_POINT('Ctrl Pts',(6.86291075501209,-0.459834002450772,
4.53124951681343));
#22509=CARTESIAN_POINT('Ctrl Pts',(6.91062659107492,-0.695543074258338,
3.90054607923755));
#22510=CARTESIAN_POINT('Ctrl Pts',(6.95834242713776,-0.292526745343327,
3.36117245204842));
#22511=CARTESIAN_POINT('Ctrl Pts',(7.00605826320061,0.379122722467859,3.40844412700009));
#22512=CARTESIAN_POINT('Ctrl Pts',(7.05377409926343,0.702617257610868,3.99895059076549));
#22513=CARTESIAN_POINT('Ctrl Pts',(7.10148993532628,0.380887926283931,4.59042078110798));
#22514=CARTESIAN_POINT('Ctrl Pts',(7.14920577138911,-0.290616845661789,
4.63969846327979));
#22515=CARTESIAN_POINT('Ctrl Pts',(7.19692160745196,-0.695243592084394,
4.10153121423426));
#22516=CARTESIAN_POINT('Ctrl Pts',(7.24463744351478,-0.461417505508394,
3.47012628326466));
#22517=CARTESIAN_POINT('Ctrl Pts',(7.29235327957764,0.196135405489393,3.32531254251214));
#22518=CARTESIAN_POINT('Ctrl Pts',(7.34006911564046,0.673574140181709,3.80007467379138));
#22519=CARTESIAN_POINT('Ctrl Pts',(7.38778495170331,0.532459385890787,4.45843130921146));
#22520=CARTESIAN_POINT('Ctrl Pts',(7.43550078776614,-0.0976210197556089,
4.69580341906706));
#22521=CARTESIAN_POINT('Ctrl Pts',(7.48321662382899,-0.638054538563543,
4.29420854311633));
#22522=CARTESIAN_POINT('Ctrl Pts',(7.53093245989182,-0.592552758097988,
3.62243743491725));
#22523=CARTESIAN_POINT('Ctrl Pts',(7.57864829595465,-0.00290066162856385,
3.29738783984629));
#22524=CARTESIAN_POINT('Ctrl Pts',(7.6263641320175,0.589415156704478,3.61755780248734));
#22525=CARTESIAN_POINT('Ctrl Pts',(7.67407996808033,0.64046196749915,4.28893031975233));
#22526=CARTESIAN_POINT('Ctrl Pts',(7.72179580414318,0.103362698669259,4.69497367861456));
#22527=CARTESIAN_POINT('Ctrl Pts',(7.769511640206,-0.528656126737314,4.46281201486565));
#22528=CARTESIAN_POINT('Ctrl Pts',(7.81722747626886,-0.675201896567852,
3.80564295658466));
#22529=CARTESIAN_POINT('Ctrl Pts',(7.86494331233168,-0.201699375449268,
3.32695496184095));
#22530=CARTESIAN_POINT('Ctrl Pts',(7.91265914839452,0.457026785680635,3.46633458176699));
#22531=CARTESIAN_POINT('Ctrl Pts',(7.96037498445737,0.696058217263005,4.09578736675475));
#22532=CARTESIAN_POINT('Ctrl Pts',(8.0080908205202,0.295888677698302,4.63727713897333));
#22533=CARTESIAN_POINT('Ctrl Pts',(8.05580665658303,-0.375999987428149,
4.59354550870361));
#22534=CARTESIAN_POINT('Ctrl Pts',(8.10352249264589,-0.702602078596463,
4.00475190491975));
#22535=CARTESIAN_POINT('Ctrl Pts',(8.1512383287087,-0.383993870066737,3.41159455373064));
#22536=CARTESIAN_POINT('Ctrl Pts',(8.19895416477156,0.287241817850264,3.35877897763223));
#22537=CARTESIAN_POINT('Ctrl Pts',(8.24667000083438,0.694698924651979,3.89480653282778));
#22538=CARTESIAN_POINT('Ctrl Pts',(8.29438583689724,0.464203319628796,4.52743486753713));
#22539=CARTESIAN_POINT('Ctrl Pts',(8.34210167296006,-0.192577336495663,
4.67571164775853));
#22540=CARTESIAN_POINT('Ctrl Pts',(8.3898175090229,-0.672511261332963,4.20347202468314));
#22541=CARTESIAN_POINT('Ctrl Pts',(8.43753334508575,-0.534867746972347,
3.54438091052171));
#22542=CARTESIAN_POINT('Ctrl Pts',(8.48524918114857,0.0939530494311211,
3.303691816829));
#22543=CARTESIAN_POINT('Ctrl Pts',(8.53296501721143,0.636495314888509,3.70243324182078));
#22544=CARTESIAN_POINT('Ctrl Pts',(8.58068085327425,0.594534138944492,4.37443479950165));
#22545=CARTESIAN_POINT('Ctrl Pts',(8.6283966893371,0.00660311512414562,
4.7025871193802));
#22546=CARTESIAN_POINT('Ctrl Pts',(8.67611252539993,-0.58739165091669,4.3855428768395));
#22547=CARTESIAN_POINT('Ctrl Pts',(8.72382836146277,-0.64197562573843,3.71444867815739));
#22548=CARTESIAN_POINT('Ctrl Pts',(8.77154419752561,-0.107023505379864,
3.30558065209521));
#22549=CARTESIAN_POINT('Ctrl Pts',(8.81926003358845,0.526209946737336,3.53440859822909));
#22550=CARTESIAN_POINT('Ctrl Pts',(8.86697586965128,0.676216707984864,4.19079629265377));
#22551=CARTESIAN_POINT('Ctrl Pts',(8.91469170571413,0.20524326135842,4.67197281575615));
#22552=CARTESIAN_POINT('Ctrl Pts',(8.96240754177695,-0.45420823024697,4.53606636251889));
#22553=CARTESIAN_POINT('Ctrl Pts',(9.0101233778398,-0.69655331512461,3.90788192013928));
#22554=CARTESIAN_POINT('Ctrl Pts',(9.05783921390263,-0.299242772872918,
3.36429092791464));
#22555=CARTESIAN_POINT('Ctrl Pts',(9.10555504996548,0.37286701214988,3.40448135822736));
#22556=CARTESIAN_POINT('Ctrl Pts',(9.15327088602831,0.702567282619003,3.99154572051203));
#22557=CARTESIAN_POINT('Ctrl Pts',(9.20098672209116,0.387089207071907,4.58637377773631));
#22558=CARTESIAN_POINT('Ctrl Pts',(9.24870255815397,-0.28385884346236,4.64272577234503));
#22559=CARTESIAN_POINT('Ctrl Pts',(9.29641839421684,-0.694134950315416,
4.10885280060212));
#22560=CARTESIAN_POINT('Ctrl Pts',(9.34413423027966,-0.46697625165475,3.47501862715065));
#22561=CARTESIAN_POINT('Ctrl Pts',(9.39185006634251,0.189013924253689,3.32328292626348));
#22562=CARTESIAN_POINT('Ctrl Pts',(9.43956590240535,0.671429705166911,3.79298692681914));
#22563=CARTESIAN_POINT('Ctrl Pts',(9.48728173846818,0.537261256551386,4.45279421778236));
#22564=CARTESIAN_POINT('Ctrl Pts',(9.53499757453101,-0.090282470782305,
4.69679361142145));
#22565=CARTESIAN_POINT('Ctrl Pts',(9.58271341059386,-0.634918416022234,
4.30091671014441));
#22566=CARTESIAN_POINT('Ctrl Pts',(9.63042924665669,-0.596499010353368,
3.62870336374299));
#22567=CARTESIAN_POINT('Ctrl Pts',(9.67814508271953,-0.0103053851599677,
3.29745743154951));
#22568=CARTESIAN_POINT('Ctrl Pts',(9.72586091878236,0.585351833794561,3.61136714997101));
#22569=CARTESIAN_POINT('Ctrl Pts',(9.77357675484522,0.643471456979869,4.28216439445919));
#22570=CARTESIAN_POINT('Ctrl Pts',(9.82129259090803,0.110681340139534,4.69384573385819));
#22571=CARTESIAN_POINT('Ctrl Pts',(9.8690084269709,-0.523749154402255,4.46835785966634));
#22572=CARTESIAN_POINT('Ctrl Pts',(9.91672426303372,-0.677212741539845,
3.81276975633088));
#22573=CARTESIAN_POINT('Ctrl Pts',(9.96444009909655,-0.208781447863971,
3.32911806666439));
#22574=CARTESIAN_POINT('Ctrl Pts',(10.0121559351594,0.451377061900895,3.4615475792254));
#22575=CARTESIAN_POINT('Ctrl Pts',(10.0598717712222,0.697029070393332,4.08844623493918));
#22576=CARTESIAN_POINT('Ctrl Pts',(10.1075876072851,0.302588558372737,4.63412335218805));
#22577=CARTESIAN_POINT('Ctrl Pts',(10.1553034433479,-0.369723682724971,
4.5974752378807));
#22578=CARTESIAN_POINT('Ctrl Pts',(10.2030192794108,-0.702512977046242,
4.01215641928927));
#22579=CARTESIAN_POINT('Ctrl Pts',(10.2507351154736,-0.390173794994359,
3.41567417381395));
#22580=CARTESIAN_POINT('Ctrl Pts',(10.2984509515364,0.280467986596366,3.3557873255338));
#22581=CARTESIAN_POINT('Ctrl Pts',(10.3461667875993,0.693551700540965,3.8874908887021));
#22582=CARTESIAN_POINT('Ctrl Pts',(10.3938826236621,0.469736216214169,4.52251329995044));
#22583=CARTESIAN_POINT('Ctrl Pts',(10.441598459725,-0.185445263282835,4.67770370795377));
#22584=CARTESIAN_POINT('Ctrl Pts',(10.4893142957878,-0.670329504065059,
4.21054837313121));
#22585=CARTESIAN_POINT('Ctrl Pts',(10.5370301318506,-0.539639846919137,
3.55004322755915));
#22586=CARTESIAN_POINT('Ctrl Pts',(10.5847459679134,0.0866093850789692,
3.30274030959437));
#22587=CARTESIAN_POINT('Ctrl Pts',(10.6324618039763,0.633323886102378,3.69574169404847));
#22588=CARTESIAN_POINT('Ctrl Pts',(10.6801776400391,0.598447317577389,4.36814816247366));
#22589=CARTESIAN_POINT('Ctrl Pts',(10.727893476102,0.0140073690254923,4.70247850861168));
#22590=CARTESIAN_POINT('Ctrl Pts',(10.7756093121648,-0.583295762033595,
4.39171203127037));
#22591=CARTESIAN_POINT('Ctrl Pts',(10.8233251482277,-0.644949419658282,
3.72123036834915));
#22592=CARTESIAN_POINT('Ctrl Pts',(10.8710409842905,-0.114336101388361,
3.30674714759503));
#22593=CARTESIAN_POINT('Ctrl Pts',(10.9187568203533,0.521273818073547,3.52888868827067));
#22594=CARTESIAN_POINT('Ctrl Pts',(10.9664726564162,0.678189969569843,4.18365899548663));
#22595=CARTESIAN_POINT('Ctrl Pts',(11.014188492479,0.212313836716152,4.66977242119035));
#22596=CARTESIAN_POINT('Ctrl Pts',(11.0619043285418,-0.44853335926228,4.54082352674158));
#22597=CARTESIAN_POINT('Ctrl Pts',(11.1096201646047,-0.697485469857315,
3.91522806604643));
#22598=CARTESIAN_POINT('Ctrl Pts',(11.1573360006675,-0.305925941288932,
3.36747997668469));
#22599=CARTESIAN_POINT('Ctrl Pts',(11.2050518367303,0.36657008644075,3.40058475730499));
#22600=CARTESIAN_POINT('Ctrl Pts',(11.2527676727932,0.702439163386103,3.98414177848112));
#22601=CARTESIAN_POINT('Ctrl Pts',(11.300483508856,0.393247548178179,4.58226164848818));
#22602=CARTESIAN_POINT('Ctrl Pts',(11.3481993449189,-0.277069341413063,
4.64568168744144));
#22603=CARTESIAN_POINT('Ctrl Pts',(11.3959151809817,-0.692949191524882,
4.11616229772746));
#22604=CARTESIAN_POINT('Ctrl Pts',(11.4436310170446,-0.47248313666557,3.47996928262364));
#22605=CARTESIAN_POINT('Ctrl Pts',(11.4913468531074,0.181871452681271,3.32132847698764));
#22606=CARTESIAN_POINT('Ctrl Pts',(11.5390626891702,0.669210688578896,3.78592217363756));
#22607=CARTESIAN_POINT('Ctrl Pts',(11.586778525233,0.54200345202451,4.44710683224685));
#22608=CARTESIAN_POINT('Ctrl Pts',(11.6344943612959,-0.082933894319074,
4.69770640718098));
#22609=CARTESIAN_POINT('Ctrl Pts',(11.6822101973587,-0.631711769407458,
4.30759145280778));
#22610=CARTESIAN_POINT('Ctrl Pts',(11.7299260334216,-0.600379006513997,
3.63501053441836));
#22611=CARTESIAN_POINT('Ctrl Pts',(11.7776418694844,-0.0177089639202829,
3.29760505835735));
#22612=CARTESIAN_POINT('Ctrl Pts',(11.8253577055473,0.581223492728864,3.60521966494218));
#22613=CARTESIAN_POINT('Ctrl Pts',(11.8730735416101,0.646409472732109,4.27536712768685));
#22614=CARTESIAN_POINT('Ctrl Pts',(11.9207893776729,0.11798768763725,4.69264072000881));
#22615=CARTESIAN_POINT('Ctrl Pts',(11.9685052137358,-0.518784006488825,
4.4738516814993));
#22616=CARTESIAN_POINT('Ctrl Pts',(12.0162210497986,-0.679148364938221,
3.81991735272367));
#22617=CARTESIAN_POINT('Ctrl Pts',(12.0639368858614,-0.215840329824027,
3.33135568986959));
#22618=CARTESIAN_POINT('Ctrl Pts',(12.1116527219243,0.445677201297934,3.45682038542343));
#22619=CARTESIAN_POINT('Ctrl Pts',(12.1593685579871,0.697922500842799,4.08109527893561));
#22620=CARTESIAN_POINT('Ctrl Pts',(12.2070843940499,0.309254828945687,4.63089912998995));
#22621=CARTESIAN_POINT('Ctrl Pts',(12.2548002301128,-0.36340631086944,4.60133860234362));
#22622=CARTESIAN_POINT('Ctrl Pts',(12.3025160661756,-0.702345843688318,
4.0195595833814));
#22623=CARTESIAN_POINT('Ctrl Pts',(12.3502319022385,-0.396310381268302,
3.41981869803717));
#22624=CARTESIAN_POINT('Ctrl Pts',(12.3979477383013,0.273663002289436,3.35286722952223));
#22625=CARTESIAN_POINT('Ctrl Pts',(12.4456635743641,0.69232743999824,3.88018774155459));
#22626=CARTESIAN_POINT('Ctrl Pts',(12.493379410427,0.475216936729713,4.51753369406595));
#22627=CARTESIAN_POINT('Ctrl Pts',(12.5410952464898,-0.178292591690169,
4.67962049203707));
#22628=CARTESIAN_POINT('Ctrl Pts',(12.5888110825527,-0.66807328977682,4.21760133486514));
#22629=CARTESIAN_POINT('Ctrl Pts',(12.6365269186155,-0.544352006232531,
3.55575552365962));
#22630=CARTESIAN_POINT('Ctrl Pts',(12.6842427546784,0.0792561005673328,
3.3018662506574));
#22631=CARTESIAN_POINT('Ctrl Pts',(12.7319585907411,0.630082110704352,3.68908394184497));
#22632=CARTESIAN_POINT('Ctrl Pts',(12.779674426804,0.60229402352211,4.36182063329482));
#22633=CARTESIAN_POINT('Ctrl Pts',(12.8273902628668,0.0214100670547408,
4.70229186986395));
#22634=CARTESIAN_POINT('Ctrl Pts',(12.8751060989297,-0.579135083425219,
4.39783767618763));
#22635=CARTESIAN_POINT('Ctrl Pts',(12.9228219349925,-0.647851575657132,
3.7280430229487));
#22636=CARTESIAN_POINT('Ctrl Pts',(12.9705377710554,-0.121635997485283,
3.30799064633195));
#22637=CARTESIAN_POINT('Ctrl Pts',(13.0182536071182,0.516279788787698,3.52342110712114));
#22638=CARTESIAN_POINT('Ctrl Pts',(13.065969443181,0.68008790103128,4.17650129834983));
#22639=CARTESIAN_POINT('Ctrl Pts',(13.1136852792439,0.219360829260397,4.66749763148232));
#22640=CARTESIAN_POINT('Ctrl Pts',(13.1614011153067,-0.44280866732052,4.54552061885334));
#22641=CARTESIAN_POINT('Ctrl Pts',(13.2091169513696,-0.698340151213866,
3.92258362801769));
#22642=CARTESIAN_POINT('Ctrl Pts',(13.2568327874324,-0.31257512890311,3.37073928277739));
#22643=CARTESIAN_POINT('Ctrl Pts',(13.3045486234952,0.36023244386594,3.39675473658331));
#22644=CARTESIAN_POINT('Ctrl Pts',(13.3522644595581,0.702233020544282,3.97673959790624));
#22645=CARTESIAN_POINT('Ctrl Pts',(13.3999802956209,0.39936220921291,4.57808484437918));
#22646=CARTESIAN_POINT('Ctrl Pts',(13.4476961316837,-0.270249063816132,
4.64856588328003));
#22647=CARTESIAN_POINT('Ctrl Pts',(13.4954119677466,-0.691686463226468,
4.123458892096));
#22648=CARTESIAN_POINT('Ctrl Pts',(13.5431278038094,-0.47793754049168,3.48497770064095));
#22649=CARTESIAN_POINT('Ctrl Pts',(13.5908436398723,0.174708779690948,3.31944941132403));
#22650=CARTESIAN_POINT('Ctrl Pts',(13.6385594759351,0.666917339243262,3.77888119920505));
#22651=CARTESIAN_POINT('Ctrl Pts',(13.6862753119979,0.54668544432619,4.44136978420615));
#22652=CARTESIAN_POINT('Ctrl Pts',(13.7339911480608,-0.075576105952426,
4.69854170502367));
#22653=CARTESIAN_POINT('Ctrl Pts',(13.7817069841236,-0.62843495524706,4.31423202967224));
#22654=CARTESIAN_POINT('Ctrl Pts',(13.8294228201864,-0.604192315423611,
3.64135824639153));
#22655=CARTESIAN_POINT('Ctrl Pts',(13.8771386562493,-0.025110575652917,
3.29783070386218));
#22656=CARTESIAN_POINT('Ctrl Pts',(13.9248544923121,0.577030592115723,3.59911603023956));
#22657=CARTESIAN_POINT('Ctrl Pts',(13.972570328375,0.649275688387581,4.26853927444071));
#22658=CARTESIAN_POINT('Ctrl Pts',(14.0202861644378,0.125280929622514,4.69135877091509));
#22659=CARTESIAN_POINT('Ctrl Pts',(14.0680020005006,-0.513761234509794,
4.47929287013608));
#22660=CARTESIAN_POINT('Ctrl Pts',(14.1157178365635,-0.681008551759042,
3.82708495184235));
#22661=CARTESIAN_POINT('Ctrl Pts',(14.1634336726263,-0.222875237264486,
3.33366758291179));
#22662=CARTESIAN_POINT('Ctrl Pts',(14.2111495086891,0.439927836986373,3.45215352543546));
#22663=CARTESIAN_POINT('Ctrl Pts',(14.258865344752,0.698738409372782,4.07373531525328));
#22664=CARTESIAN_POINT('Ctrl Pts',(14.3065811808148,0.315886748959774,4.62760483051036));
#22665=CARTESIAN_POINT('Ctrl Pts',(14.3542970168777,-0.357048573565392,
4.60513517296818));
#22666=CARTESIAN_POINT('Ctrl Pts',(14.4020128529405,-0.702100697086982,
4.02696057488784));
#22667=CARTESIAN_POINT('Ctrl Pts',(14.4497286890033,-0.402402947265751,
3.42402766604624));
#22668=CARTESIAN_POINT('Ctrl Pts',(14.4974445250662,0.266827620794843,3.35001901394789));
#22669=CARTESIAN_POINT('Ctrl Pts',(14.545160361129,0.691026279008849,3.87289790258421));
#22670=CARTESIAN_POINT('Ctrl Pts',(14.5928761971919,0.480644872403009,4.51249660299459));
#22671=CARTESIAN_POINT('Ctrl Pts',(14.6405920332547,-0.171120116202498,
4.6814617871012));
#22672=CARTESIAN_POINT('Ctrl Pts',(14.6883078693176,-0.665742869077823,
4.22463012647536));
#22673=CARTESIAN_POINT('Ctrl Pts',(14.7360237053803,-0.549003701508229,
3.56151716432844));
#22674=CARTESIAN_POINT('Ctrl Pts',(14.7837395414432,0.0718940126641393,
3.30106973710437));
#22675=CARTESIAN_POINT('Ctrl Pts',(14.831455377506,0.626770348775451,3.68246072472179));
#22676=CARTESIAN_POINT('Ctrl Pts',(14.8791712135689,0.606073829504824,4.35545291479698));
#22677=CARTESIAN_POINT('Ctrl Pts',(14.9268870496317,0.0288103869553486,
4.70202722386799));
#22678=CARTESIAN_POINT('Ctrl Pts',(14.9746028856946,-0.574910077240004,
4.4039191311837));
#22679=CARTESIAN_POINT('Ctrl Pts',(15.0223187217574,-0.650681771377263,
3.73488588523872));
#22680=CARTESIAN_POINT('Ctrl Pts',(15.0700345578202,-0.128922382832804,
3.30931101018402));
#22681=CARTESIAN_POINT('Ctrl Pts',(15.1177503938831,0.511228413592865,3.51800646209349));
#22682=CARTESIAN_POINT('Ctrl Pts',(15.1654662299459,0.681910291555949,4.16932399628639));
#22683=CARTESIAN_POINT('Ctrl Pts',(15.2131820660088,0.226383456244684,4.6651486993049));
#22684=CARTESIAN_POINT('Ctrl Pts',(15.2608979020716,-0.437034790293287,
4.55015711712348));
#22685=CARTESIAN_POINT('Ctrl Pts',(15.3086137381344,-0.699117264260319,
3.92994778903219));
#22686=CARTESIAN_POINT('Ctrl Pts',(15.3563295741972,-0.319189597155267,
3.37406848416447));
#22687=CARTESIAN_POINT('Ctrl Pts',(15.4040454102601,0.353854788380711,3.39299172148285));
#22688=CARTESIAN_POINT('Ctrl Pts',(15.4517612463229,0.70194887699091,3.96934000098645));
#22689=CARTESIAN_POINT('Ctrl Pts',(15.4994770823858,0.40543251098856,4.57384382934891));
#22690=CARTESIAN_POINT('Ctrl Pts',(15.5471929184486,-0.263398768235635,
4.65137803949801));
#22691=CARTESIAN_POINT('Ctrl Pts',(15.5949087545115,-0.690346905678043,
4.13074177323664));
#22692=CARTESIAN_POINT('Ctrl Pts',(15.6426245905743,-0.483338857283784,
3.4900433248913));
#22693=CARTESIAN_POINT('Ctrl Pts',(15.6903404266371,0.167526700878456,3.31764593799033));
#22694=CARTESIAN_POINT('Ctrl Pts',(15.7380562627,0.664549911894371,3.77186478559966));
#22695=CARTESIAN_POINT('Ctrl Pts',(15.7857720987628,0.551306713402943,4.43558371090429));
#22696=CARTESIAN_POINT('Ctrl Pts',(15.8334879348256,-0.0682099229505586,
4.69929941216862));
#22697=CARTESIAN_POINT('Ctrl Pts',(15.8812037708885,-0.625088337514006,
4.32083770313399));
#22698=CARTESIAN_POINT('Ctrl Pts',(15.9289196069513,-0.607938513517956,
3.64774579458877));
#22699=CARTESIAN_POINT('Ctrl Pts',(15.9766354430142,-0.0325093982219456,
3.29813434300035));
#22700=CARTESIAN_POINT('Ctrl Pts',(16.024351279077,0.572773597682653,3.59305692382598));
#22701=CARTESIAN_POINT('Ctrl Pts',(16.0720671151399,0.652069785580651,4.2616815931263));
#22702=CARTESIAN_POINT('Ctrl Pts',(16.1197829512026,0.132560255996602,4.69000002896988));
#22703=CARTESIAN_POINT('Ctrl Pts',(16.1674987872655,-0.508681396370837,
4.48468082119526));
#22704=CARTESIAN_POINT('Ctrl Pts',(16.2152146233283,-0.682793095381579,
3.83427175754402));
#22705=CARTESIAN_POINT('Ctrl Pts',(16.2629304593912,-0.229885388781225,
3.33605348899688));
#22706=CARTESIAN_POINT('Ctrl Pts',(16.310646295454,0.434129607578297,3.44754751763412));
#22707=CARTESIAN_POINT('Ctrl Pts',(16.3583621315168,0.699476705356048,4.06636716140204));
#22708=CARTESIAN_POINT('Ctrl Pts',(16.4060779675797,0.322483581772784,4.62424081966442));
#22709=CARTESIAN_POINT('Ctrl Pts',(16.4537938036425,-0.350651177000141,
4.60886452804932));
#22710=CARTESIAN_POINT('Ctrl Pts',(16.5015096397054,-0.701777564471952,
4.03435857174156));
#22711=CARTESIAN_POINT('Ctrl Pts',(16.5492254757682,-0.408450816253369,
3.42830061032894));
#22712=CARTESIAN_POINT('Ctrl Pts',(16.596941311831,0.259962601354342,3.34724299517707));
#22713=CARTESIAN_POINT('Ctrl Pts',(16.6446571478939,0.689648362099571,3.86562218151166));
#22714=CARTESIAN_POINT('Ctrl Pts',(16.6923729839567,0.486019420324727,4.50740258623259));
#22715=CARTESIAN_POINT('Ctrl Pts',(16.7400888200196,-0.163928633504336,
4.6832273886238));
#22716=CARTESIAN_POINT('Ctrl Pts',(16.7878046560824,-0.663338500820136,
4.23163396723712));
#22717=CARTESIAN_POINT('Ctrl Pts',(16.8355204921452,-0.553594416058007,
3.56732750958986));
#22718=CARTESIAN_POINT('Ctrl Pts',(16.8832363282081,0.064523939115192,3.30035085740826));
#22719=CARTESIAN_POINT('Ctrl Pts',(16.9309521642709,0.623388968170475,3.67587277835446));
#22720=CARTESIAN_POINT('Ctrl Pts',(16.9786680003338,0.609786315682611,4.34904571427615));
#22721=CARTESIAN_POINT('Ctrl Pts',(17.0263838363966,0.0362075067348799,
4.70168460001938));
#22722=CARTESIAN_POINT('Ctrl Pts',(17.0740996724594,-0.570621212771584,
4.40995572075944));
#22723=CARTESIAN_POINT('Ctrl Pts',(17.1218155085223,-0.653439692453966,
3.74175819514654));
#22724=CARTESIAN_POINT('Ctrl Pts',(17.1695313445851,-0.136194448093839,
3.31070809249149));
#22725=CARTESIAN_POINT('Ctrl Pts',(17.2172471806479,0.50612025357182,3.51264535462077));
#22726=CARTESIAN_POINT('Ctrl Pts',(17.2649630167108,0.683656938721366,4.16212788651693));
#22727=CARTESIAN_POINT('Ctrl Pts',(17.3126788527736,0.233380937628925,4.66272588556639));
#22728=CARTESIAN_POINT('Ctrl Pts',(17.3603946888365,-0.431212369515449,
4.55473250655174));
#22729=CARTESIAN_POINT('Ctrl Pts',(17.4081105248993,-0.699816722678643,
3.93731973111387));
#22730=CARTESIAN_POINT('Ctrl Pts',(17.4558263609621,-0.325768611341644,
3.37746721105403));
#22731=CARTESIAN_POINT('Ctrl Pts',(17.503542197025,0.347437828384778,3.38929612998149));
#22732=CARTESIAN_POINT('Ctrl Pts',(17.5512580330878,0.701586764287296,3.96194380963385));
#22733=CARTESIAN_POINT('Ctrl Pts',(17.5989738691507,0.411457779244836,4.56953907446917));
#22734=CARTESIAN_POINT('Ctrl Pts',(17.6466897052135,-0.256519215569882,
4.65411784373439));
#22735=CARTESIAN_POINT('Ctrl Pts',(17.6944055412764,-0.688930667671302,
4.13801013220155));
#22736=CARTESIAN_POINT('Ctrl Pts',(17.7421213773391,-0.488686487089258,
3.49516559270919));
#22737=CARTESIAN_POINT('Ctrl Pts',(17.789837213402,0.160326013994967,3.3159182573078));
#22738=CARTESIAN_POINT('Ctrl Pts',(17.8375530494648,0.662108669494809,3.76487371217125));
#22739=CARTESIAN_POINT('Ctrl Pts',(17.8852688855277,0.555866745946156,4.42974925503083));
#22740=CARTESIAN_POINT('Ctrl Pts',(17.9329847215905,-0.060836163514142,
4.69997944445332));
#22741=CARTESIAN_POINT('Ctrl Pts',(17.9807005576534,-0.621672287934692,
4.32740773946617));
#22742=CARTESIAN_POINT('Ctrl Pts',(18.0284163937162,-0.611617184687133,
3.65417246951162));
#22743=CARTESIAN_POINT('Ctrl Pts',(18.0761322297791,-0.0399046098013318,
3.29851594204507));
#22744=CARTESIAN_POINT('Ctrl Pts',(18.1238480658419,0.568452982276385,3.58704301871817));
#22745=CARTESIAN_POINT('Ctrl Pts',(18.1715639019047,0.65479145395626,4.25479484546229));
#22746=CARTESIAN_POINT('Ctrl Pts',(18.2192797379675,0.139824858206545,4.68856464509573));
#22747=CARTESIAN_POINT('Ctrl Pts',(18.2669955740304,-0.503545056316242,
4.49001493620888));
#22748=CARTESIAN_POINT('Ctrl Pts',(18.3147114100932,-0.684501797587214,
3.84147697155243));
#22749=CARTESIAN_POINT('Ctrl Pts',(18.3624272461561,-0.236870005719869,
3.33851314310973));
#22750=CARTESIAN_POINT('Ctrl Pts',(18.4101430822189,0.42828315711354,3.44300287363294));
#22751=CARTESIAN_POINT('Ctrl Pts',(18.4578589182817,0.70013730678616,4.05899163580144));
#22752=CARTESIAN_POINT('Ctrl Pts',(18.5055747543446,0.32904459463985,4.62080747111051));
#22753=CARTESIAN_POINT('Ctrl Pts',(18.5532905904074,-0.34421483176614,4.61252625334797));
#22754=CARTESIAN_POINT('Ctrl Pts',(18.6010064264702,-0.701376481735239,
4.0417527522082));
#22755=CARTESIAN_POINT('Ctrl Pts',(18.6487222625331,-0.414453316462639,
3.43263705626685));
#22756=CARTESIAN_POINT('Ctrl Pts',(18.6964380985959,0.253068706501803,3.34453948155689));
#22757=CARTESIAN_POINT('Ctrl Pts',(18.7441539346588,0.68819384232267,3.85836138648927));
#22758=CARTESIAN_POINT('Ctrl Pts',(18.7918697707216,0.491339983515996,4.50225220959958));
#22759=CARTESIAN_POINT('Ctrl Pts',(18.8395856067844,-0.156718942392259,
4.68491710048942));
#22760=CARTESIAN_POINT('Ctrl Pts',(18.8873014428473,-0.660860452068119,
4.23861207919858));
#22761=CARTESIAN_POINT('Ctrl Pts',(18.9350172789101,-0.558123639969822,
3.57318591405529));
#22762=CARTESIAN_POINT('Ctrl Pts',(18.9827331149729,0.0571466985584877,
3.29970969142451));
#22763=CARTESIAN_POINT('Ctrl Pts',(19.0304489510358,0.619938344467307,3.66932083449001));
#22764=CARTESIAN_POINT('Ctrl Pts',(19.0781647870986,0.613431069708698,4.3425997434341));
#22765=CARTESIAN_POINT('Ctrl Pts',(19.1258806231615,0.0436006047213211,
4.70126403633668));
#22766=CARTESIAN_POINT('Ctrl Pts',(19.1735964592243,-0.566268966340429,
4.41594677447179));
#22767=CARTESIAN_POINT('Ctrl Pts',(19.2213122952871,-0.656125032675529,
3.74865918919138));
#22768=CARTESIAN_POINT('Ctrl Pts',(19.26902813135,-0.143451385285705,3.31218173833215));
#22769=CARTESIAN_POINT('Ctrl Pts',(19.3167439674128,0.500955875668841,3.50733837970023));
#22770=CARTESIAN_POINT('Ctrl Pts',(19.3644598034757,0.68532764936022,4.15491376927485));
#22771=CARTESIAN_POINT('Ctrl Pts',(19.4121756395385,0.240352494576274,4.66022945763735));
#22772=CARTESIAN_POINT('Ctrl Pts',(19.4598914756013,-0.425342048711971,
4.55924628221868));
#22773=CARTESIAN_POINT('Ctrl Pts',(19.5076073116642,-0.700438454444525,
3.94469862920436));
#22774=CARTESIAN_POINT('Ctrl Pts',(19.555323147727,-0.332311429993836,3.3809350976725));
#22775=CARTESIAN_POINT('Ctrl Pts',(19.6030389837899,0.340982256434611,3.38566835039883));
#22776=CARTESIAN_POINT('Ctrl Pts',(19.6507548198527,0.701146760813864,3.95455188724214));
#22777=CARTESIAN_POINT('Ctrl Pts',(19.6984706559155,0.417437272672218,4.56517097885182));
#22778=CARTESIAN_POINT('Ctrl Pts',(19.7461864919784,-0.249611033919464,
4.6567851409082));
#22779=CARTESIAN_POINT('Ctrl Pts',(19.7939023280412,-0.687438163400574,
4.14526287985386));
#22780=CARTESIAN_POINT('Ctrl Pts',(19.841618164104,-0.493979350866992,3.5003444672369));
#22781=CARTESIAN_POINT('Ctrl Pts',(19.8893340001669,0.153106602982307,3.31426555646693));
#22782=CARTESIAN_POINT('Ctrl Pts',(19.9370498362297,0.659595612567133,3.75791065255607));
#22783=CARTESIAN_POINT('Ctrl Pts',(19.9847656722925,0.560361770063263,4.42386348253578));
#22784=CARTESIAN_POINT('Ctrl Pts',(20.0324815083554,-0.0534494809679074,
4.70058849011268));
#22785=CARTESIAN_POINT('Ctrl Pts',(20.0801973444182,-0.618198828117398,
4.33392863744107));
#22786=CARTESIAN_POINT('Ctrl Pts',(20.1279131804811,-0.615205937201001,
3.66066167313574));
#22787=CARTESIAN_POINT('Ctrl Pts',(20.1756290165439,-0.0473369003220797,
3.29892991724937));
#22788=CARTESIAN_POINT('Ctrl Pts',(20.2233448526068,0.564147630203746,3.58116102158214));
#22789=CARTESIAN_POINT('Ctrl Pts',(20.2710606886696,0.657292163719816,4.24771695100806));
#22790=CARTESIAN_POINT('Ctrl Pts',(20.3187765247324,0.147355317357748,4.68736342730055));
#22791=CARTESIAN_POINT('Ctrl Pts',(20.3664923607953,-0.498896366832293,
4.49468216892218));
#22792=CARTESIAN_POINT('Ctrl Pts',(20.4062555575143,-0.653992183610565,
3.9575054511282));
#22793=CARTESIAN_POINT('Ctrl Pts',(20.4380661148895,-0.465699721472375,
3.59327933193152));
#22794=CARTESIAN_POINT('Ctrl Pts',(20.461924032921,-0.215665100260693,3.41899970433759));
#22795=CARTESIAN_POINT('Ctrl Pts',(20.4857819509523,0.0900520562992202,
3.38718375849312));
#22796=CARTESIAN_POINT('Ctrl Pts',(20.5096398689838,0.372154449079436,3.50499792242313));
#22797=CARTESIAN_POINT('Ctrl Pts',(20.5334977870152,0.564103623124681,3.74397162737493));
#22798=CARTESIAN_POINT('Ctrl Pts',(20.5573557050466,0.61766411855396,4.04548854604559));
#22799=CARTESIAN_POINT('Ctrl Pts',(20.581213623078,0.520427284318709,4.33591550271974));
#22800=CARTESIAN_POINT('Ctrl Pts',(20.6050715411094,0.295805552416038,4.5441843692251));
#22801=CARTESIAN_POINT('Ctrl Pts',(20.6289294591409,-0.00108183093298003,
4.61939465531364));
#22802=CARTESIAN_POINT('Ctrl Pts',(20.6527873771723,-0.297740088546312,
4.543141139652));
#22803=CARTESIAN_POINT('Ctrl Pts',(20.6766452952037,-0.521574030203058,
4.33407743490148));
#22804=CARTESIAN_POINT('Ctrl Pts',(20.7005032132351,-0.617878846294169,
4.04332131262121));
#22805=CARTESIAN_POINT('Ctrl Pts',(20.7243611312665,-0.563090193646282,
3.74197268265107));
#22806=CARTESIAN_POINT('Ctrl Pts',(20.748219049298,-0.370613436173077,3.50371837193987));
#22807=CARTESIAN_POINT('Ctrl Pts',(20.7720769673294,-0.0875101228827464,
3.38681864340431));
#22808=CARTESIAN_POINT('Ctrl Pts',(20.7959348853608,0.216991017820888,3.41985835035499));
#22809=CARTESIAN_POINT('Ctrl Pts',(20.8197928033922,0.468432357761717,3.59475855107288));
#22810=CARTESIAN_POINT('Ctrl Pts',(20.8436507214236,0.605329007232586,3.86875129405724));
#22811=CARTESIAN_POINT('Ctrl Pts',(20.8675086394551,0.594206341669864,4.17483793696784));
#22812=CARTESIAN_POINT('Ctrl Pts',(20.8913665574864,0.437783978244149,4.43817193323088));
#22813=CARTESIAN_POINT('Ctrl Pts',(20.9152244755179,0.174311539695801,4.5943609607934));
#22814=CARTESIAN_POINT('Ctrl Pts',(20.9390823935493,-0.13178483570001,4.60521254097096));
#22815=CARTESIAN_POINT('Ctrl Pts',(20.9629403115808,-0.405656219889506,
4.46807317049539));
#22816=CARTESIAN_POINT('Ctrl Pts',(20.9867982296121,-0.580333613298163,
4.21647715910241));
#22817=CARTESIAN_POINT('Ctrl Pts',(21.0106561476436,-0.613103627724174,
3.91194658594648));
#22818=CARTESIAN_POINT('Ctrl Pts',(21.034514065675,-0.495953105920446,3.62894747086441));
#22819=CARTESIAN_POINT('Ctrl Pts',(21.0583719837064,-0.257528539509485,
3.43668080652407));
#22820=CARTESIAN_POINT('Ctrl Pts',(21.0822299017379,0.0438687693677006,
3.38216102944232));
#22821=CARTESIAN_POINT('Ctrl Pts',(21.1060878197692,0.334538969374667,3.47871971028568));
#22822=CARTESIAN_POINT('Ctrl Pts',(21.1299457378007,0.543405278604256,3.7027456213393));
#22823=CARTESIAN_POINT('Ctrl Pts',(21.153803655832,0.619394195209021,3.99945832503004));
#22824=CARTESIAN_POINT('Ctrl Pts',(21.1776615738635,0.543924359096133,4.29630348300169));
#22825=CARTESIAN_POINT('Ctrl Pts',(21.2015194918949,0.33545020099803,4.52069436823682));
#22826=CARTESIAN_POINT('Ctrl Pts',(21.2253774099264,0.0449493312674926,
4.61776129700707));
#22827=CARTESIAN_POINT('Ctrl Pts',(21.2492353279577,-0.256542874348706,
4.56376876117982));
#22828=CARTESIAN_POINT('Ctrl Pts',(21.2730932459892,-0.495303359101402,
4.37191940649105));
#22829=CARTESIAN_POINT('Ctrl Pts',(21.2969511640206,-0.612948680759938,
4.08912562603418));
#22830=CARTESIAN_POINT('Ctrl Pts',(21.320809082052,-0.580711353586496,3.78453820227854));
#22831=CARTESIAN_POINT('Ctrl Pts',(21.3446670000834,-0.406474282201139,
3.53263705712739));
#22832=CARTESIAN_POINT('Ctrl Pts',(21.3685249181149,-0.132843176680646,
3.39501888221951));
#22833=CARTESIAN_POINT('Ctrl Pts',(21.3923828361463,0.17327170411384,3.40533506996376));
#22834=CARTESIAN_POINT('Ctrl Pts',(21.4162407541777,0.437016933425986,3.56106303144932));
#22835=CARTESIAN_POINT('Ctrl Pts',(21.4400986722091,0.593899618413251,3.82412303814848));
#22836=CARTESIAN_POINT('Ctrl Pts',(21.4639565902405,0.605557669197671,4.13018975281259));
#22837=CARTESIAN_POINT('Ctrl Pts',(21.4878145082719,0.469140374803543,4.40442152661638));
#22838=CARTESIAN_POINT('Ctrl Pts',(21.5116724263034,0.218005479642704,4.57976122094124));
#22839=CARTESIAN_POINT('Ctrl Pts',(21.5355303443348,-0.0864376936408111,
4.61333350436739));
#22840=CARTESIAN_POINT('Ctrl Pts',(21.5593882623662,-0.369744496313637,
4.49692903910649));
#22841=CARTESIAN_POINT('Ctrl Pts',(21.5832461803976,-0.562638697999917,
4.2590118877088));
#22842=CARTESIAN_POINT('Ctrl Pts',(21.607104098429,-0.617952412054802,3.95775927442416));
#22843=CARTESIAN_POINT('Ctrl Pts',(21.6309620164605,-0.522159928676552,
3.66683566915707));
#22844=CARTESIAN_POINT('Ctrl Pts',(21.6548199344919,-0.298685119385998,
3.45737981799522));
#22845=CARTESIAN_POINT('Ctrl Pts',(21.6786778525233,-0.00217366238626178,
3.38060938201055));
#22846=CARTESIAN_POINT('Ctrl Pts',(21.7025357705547,0.294869314276287,3.45529682398599));
#22847=CARTESIAN_POINT('Ctrl Pts',(21.7263936885862,0.519808711519421,3.66317902991346));
#22848=CARTESIAN_POINT('Ctrl Pts',(21.7502516066175,0.617640719491047,3.95342313784609));
#22849=CARTESIAN_POINT('Ctrl Pts',(21.774109524649,0.564442747351711,4.25505655730362));
#22850=CARTESIAN_POINT('Ctrl Pts',(21.7979674426804,0.373223148373148,4.49432170089927));
#22851=CARTESIAN_POINT('Ctrl Pts',(21.8218253607118,0.0907403232229101,
4.61271172357229));
#22852=CARTESIAN_POINT('Ctrl Pts',(21.8456832787432,-0.213930982672105,
4.58127703989962));
#22853=CARTESIAN_POINT('Ctrl Pts',(21.8695411967746,-0.466290335940828,
4.40770428630285));
#22854=CARTESIAN_POINT('Ctrl Pts',(21.8933991148061,-0.604629000578284,
4.13443672906324));
#22855=CARTESIAN_POINT('Ctrl Pts',(21.9172570328375,-0.595119404811066,
3.82829572958469));
#22856=CARTESIAN_POINT('Ctrl Pts',(21.9411149508689,-0.440086903840403,
3.56414110135311));
#22857=CARTESIAN_POINT('Ctrl Pts',(21.9649728689003,-0.177441167154219,
3.40656584639871));
#22858=CARTESIAN_POINT('Ctrl Pts',(21.9888307869318,0.128593768301574,3.39410140682164));
#22859=CARTESIAN_POINT('Ctrl Pts',(22.0126887049631,0.403184024583593,3.52979567762293));
#22860=CARTESIAN_POINT('Ctrl Pts',(22.0365466229946,0.579184804342829,3.7804677133541));
#22861=CARTESIAN_POINT('Ctrl Pts',(22.060404541026,0.613559122762511,4.08482137310942));
#22862=CARTESIAN_POINT('Ctrl Pts',(22.0842624590574,0.497901522652627,4.36843389665204));
#22863=CARTESIAN_POINT('Ctrl Pts',(22.1081203770888,0.260493437687466,4.56195429652472));
#22864=CARTESIAN_POINT('Ctrl Pts',(22.1319782951203,-0.0406123884881684,
4.61806156357065));
#22865=CARTESIAN_POINT('Ctrl Pts',(22.1558362131517,-0.33178737942464,4.52303594266224));
#22866=CARTESIAN_POINT('Ctrl Pts',(22.1796941311831,-0.541831318374727,
4.30011378656432));
#22867=CARTESIAN_POINT('Ctrl Pts',(22.2035520492145,-0.619382740812877,
4.00380563470766));
#22868=CARTESIAN_POINT('Ctrl Pts',(22.2274099672459,-0.545478211438426,
3.70656690151735));
#22869=CARTESIAN_POINT('Ctrl Pts',(22.2512678852774,-0.338189400908512,
3.48108055383335));
#22870=CARTESIAN_POINT('Ctrl Pts',(22.2751258033088,-0.0482040696311437,
3.38248414587532));
#22871=CARTESIAN_POINT('Ctrl Pts',(22.2989837213402,0.253568469476171,3.43488718493857));
#22872=CARTESIAN_POINT('Ctrl Pts',(22.3228416393716,0.493336611197201,3.62547570084914));
#22873=CARTESIAN_POINT('Ctrl Pts',(22.346699557403,0.612470512379129,3.90764560936005));
#22874=CARTESIAN_POINT('Ctrl Pts',(22.3705574754344,0.581838691587799,4.21239868278141));
#22875=CARTESIAN_POINT('Ctrl Pts',(22.3944153934659,0.408931458591185,4.46521449128699));
#22876=CARTESIAN_POINT('Ctrl Pts',(22.4182733114973,0.13602935083686,4.60427268703701));
#22877=CARTESIAN_POINT('Ctrl Pts',(22.4421312295287,-0.170135649772668,
4.59556974592947));
#22878=CARTESIAN_POINT('Ctrl Pts',(22.4659891475601,-0.434697828443077,
4.44123378804823));
#22879=CARTESIAN_POINT('Ctrl Pts',(22.4898470655916,-0.592964587096883,
4.17900413283907));
#22880=CARTESIAN_POINT('Ctrl Pts',(22.513704983623,-0.606235276705168,3.87300312362118));
#22881=CARTESIAN_POINT('Ctrl Pts',(22.5375629016543,-0.471265070143009,
3.59805624874041));
#22882=CARTESIAN_POINT('Ctrl Pts',(22.5614208196858,-0.22105744785653,3.4213956854475));
#22883=CARTESIAN_POINT('Ctrl Pts',(22.5852787377172,0.0832042338527798,
3.38621941950615));
#22884=CARTESIAN_POINT('Ctrl Pts',(22.6091366557487,0.36712117327337,3.50112963696785));
#22885=CARTESIAN_POINT('Ctrl Pts',(22.63299457378,0.561265174232679,3.7380264683998));
#22886=CARTESIAN_POINT('Ctrl Pts',(22.6568524918115,0.618167971965146,4.03898443479498));
#22887=CARTESIAN_POINT('Ctrl Pts',(22.6807104098429,0.523905402647805,4.33040686810369));
#22888=CARTESIAN_POINT('Ctrl Pts',(22.7045683278744,0.301545895245711,4.54104106792393));
#22889=CARTESIAN_POINT('Ctrl Pts',(22.7284262459057,0.00542710047790416,
4.61936606261506));
#22890=CARTESIAN_POINT('Ctrl Pts',(22.7522841639372,-0.291974666000346,
4.54625809930836));
#22891=CARTESIAN_POINT('Ctrl Pts',(22.7761420819686,-0.518067845615496,
4.33953802216683));
#22892=CARTESIAN_POINT('Ctrl Pts',(22.7920473606562,-0.584213376873476,
4.14642833911731));
#22893=CARTESIAN_POINT('Ctrl Pts',(22.8,-0.592174260192535,4.04779597854866));
#22894=CARTESIAN_POINT('Ctrl Pts',(3.96816317011931,-0.282716247115855,
3.54616445487434));
#22895=CARTESIAN_POINT('Ctrl Pts',(3.97611580946312,-0.207125539895404,
3.49907532469992));
#22896=CARTESIAN_POINT('Ctrl Pts',(3.99202108815073,-0.0320395462633344,
3.44344227840288));
#22897=CARTESIAN_POINT('Ctrl Pts',(4.01587900618214,0.238586678544665,3.49618207793602));
#22898=CARTESIAN_POINT('Ctrl Pts',(4.03973692421357,0.450798406251909,3.67207593825259));
#22899=CARTESIAN_POINT('Ctrl Pts',(4.06359484224498,0.552814952159096,3.92817792166325));
#22900=CARTESIAN_POINT('Ctrl Pts',(4.0874527602764,0.519633627921064,4.20183097195279));
#22901=CARTESIAN_POINT('Ctrl Pts',(4.11131067830782,0.359398059257131,4.42613686623617));
#22902=CARTESIAN_POINT('Ctrl Pts',(4.13516859633924,0.11127440638865,4.54623750576341));
#22903=CARTESIAN_POINT('Ctrl Pts',(4.15902651437066,-0.164055973910312,
4.53276988152218));
#22904=CARTESIAN_POINT('Ctrl Pts',(4.18288443240208,-0.399271733473279,
4.38902461621758));
#22905=CARTESIAN_POINT('Ctrl Pts',(4.2067423504335,-0.536853866020863,4.15015270818839));
#22906=CARTESIAN_POINT('Ctrl Pts',(4.23060026846491,-0.543161034884179,
3.87456412255522));
#22907=CARTESIAN_POINT('Ctrl Pts',(4.25445818649634,-0.416650307492554,
3.62964815836115));
#22908=CARTESIAN_POINT('Ctrl Pts',(4.27831610452775,-0.188257351244862,
3.47529323740438));
#22909=CARTESIAN_POINT('Ctrl Pts',(4.30217402255918,0.0861697193074588,
3.44924344981891));
#22910=CARTESIAN_POINT('Ctrl Pts',(4.32603194059059,0.339525912432458,3.55786862136322));
#22911=CARTESIAN_POINT('Ctrl Pts',(4.34988985862202,0.509858789389686,3.77460696883261));
#22912=CARTESIAN_POINT('Ctrl Pts',(4.37374777665342,0.555517294574929,4.0464600464808));
#22913=CARTESIAN_POINT('Ctrl Pts',(4.39760569468486,0.465336694276122,4.30695238014399));
#22914=CARTESIAN_POINT('Ctrl Pts',(4.42146361271626,0.261368594047533,4.4923864940975));
#22915=CARTESIAN_POINT('Ctrl Pts',(4.4453215307477,-0.00651124555331369,
4.55741869872598));
#22916=CARTESIAN_POINT('Ctrl Pts',(4.4691794487791,-0.272798909000308,4.48614684730087));
#22917=CARTESIAN_POINT('Ctrl Pts',(4.49303736681053,-0.472379807908186,
4.29599884956661));
#22918=CARTESIAN_POINT('Ctrl Pts',(4.51689528484195,-0.55645097662433,4.03347107014466));
#22919=CARTESIAN_POINT('Ctrl Pts',(4.54075320287336,-0.504454724024634,
3.76275870240323));
#22920=CARTESIAN_POINT('Ctrl Pts',(4.56461112090479,-0.329105550388866,
3.55005829421323));
#22921=CARTESIAN_POINT('Ctrl Pts',(4.5884690389362,-0.0732811049967102,
3.44738088927219));
#22922=CARTESIAN_POINT('Ctrl Pts',(4.61232695696762,0.200462566687888,3.47983390993684));
#22923=CARTESIAN_POINT('Ctrl Pts',(4.63618487499904,0.425187680335341,3.63948170866684));
#22924=CARTESIAN_POINT('Ctrl Pts',(4.66004279303046,0.54594282425631,3.88728604994618));
#22925=CARTESIAN_POINT('Ctrl Pts',(4.68390071106188,0.533200076465109,4.16265202228146));
#22926=CARTESIAN_POINT('Ctrl Pts',(4.7077586290933,0.390075385898422,4.39824514461603));
#22927=CARTESIAN_POINT('Ctrl Pts',(4.73161654712472,0.151566638040082,4.53645648111246));
#22928=CARTESIAN_POINT('Ctrl Pts',(4.75547446515614,-0.124004281411749,
4.54348959519552));
#22929=CARTESIAN_POINT('Ctrl Pts',(4.77933238318755,-0.369252776249408,
4.41762469889406));
#22930=CARTESIAN_POINT('Ctrl Pts',(4.80319030121898,-0.524208909050512,
4.18963918784455));
#22931=CARTESIAN_POINT('Ctrl Pts',(4.82704821925039,-0.550981684424725,
3.91528172969931));
#22932=CARTESIAN_POINT('Ctrl Pts',(4.85090613728181,-0.443024429517375,
3.66164019632193));
#22933=CARTESIAN_POINT('Ctrl Pts',(4.87476405531323,-0.226735633849849,
3.49073685167984));
#22934=CARTESIAN_POINT('Ctrl Pts',(4.89862197334465,0.0449962004486201,
3.44436221885167));
#22935=CARTESIAN_POINT('Ctrl Pts',(4.92247989137607,0.305725238065515,3.53385615878353));
#22936=CARTESIAN_POINT('Ctrl Pts',(4.94633780940749,0.491696127187109,3.73733496539613));
#22937=CARTESIAN_POINT('Ctrl Pts',(4.9701957274389,0.557433919677865,4.00504252782125));
#22938=CARTESIAN_POINT('Ctrl Pts',(4.99405364547033,0.486863934612277,4.27151705483839));
#22939=CARTESIAN_POINT('Ctrl Pts',(5.01791156350174,0.297242455626679,4.47159826597145));
#22940=CARTESIAN_POINT('Ctrl Pts',(5.04176948153317,0.0349370995184326,
4.55636085499566));
#22941=CARTESIAN_POINT('Ctrl Pts',(5.06562739956458,-0.235911329089554,
4.505078060008));
#22942=CARTESIAN_POINT('Ctrl Pts',(5.08948531759601,-0.449073011639563,
4.33028992129829));
#22943=CARTESIAN_POINT('Ctrl Pts',(5.11334323562741,-0.552424110340463,
4.07473689991432));
#22944=CARTESIAN_POINT('Ctrl Pts',(5.13720115365885,-0.520692466332485,
3.80090867070902));
#22945=CARTESIAN_POINT('Ctrl Pts',(5.16105907169026,-0.361637330928202,
3.57576369465428));
#22946=CARTESIAN_POINT('Ctrl Pts',(5.18491698972168,-0.114152017308863,
3.45435605122152));
#22947=CARTESIAN_POINT('Ctrl Pts',(5.2087749077531,0.161246573981014,3.46637321630784));
#22948=CARTESIAN_POINT('Ctrl Pts',(5.23263282578452,0.397215985664045,3.60887666570863));
#22949=CARTESIAN_POINT('Ctrl Pts',(5.25649074381594,0.536055268906009,3.84702042432939));
#22950=CARTESIAN_POINT('Ctrl Pts',(5.28034866184735,0.543814437048104,4.12257185628156));
#22951=CARTESIAN_POINT('Ctrl Pts',(5.30420657987878,0.418596162124088,4.3681511305826));
#22952=CARTESIAN_POINT('Ctrl Pts',(5.32806449791019,0.191019723230217,4.5237074252207));
#22953=CARTESIAN_POINT('Ctrl Pts',(5.35192241594161,-0.0832662412662402,
4.55120298888854));
#22954=CARTESIAN_POINT('Ctrl Pts',(5.37578033397303,-0.337191341646214,
4.44391440730515));
#22955=CARTESIAN_POINT('Ctrl Pts',(5.39963825200445,-0.508663974085987,
4.22807666114996));
#22956=CARTESIAN_POINT('Ctrl Pts',(5.42349617003587,-0.555754409133215,
3.95646795866016));
#22957=CARTESIAN_POINT('Ctrl Pts',(5.4473540880673,-0.466947752701331,3.69550402606682));
#22958=CARTESIAN_POINT('Ctrl Pts',(5.47121200609871,-0.263959651332346,
3.50899765340418));
#22959=CARTESIAN_POINT('Ctrl Pts',(5.49506992413013,0.00357377490351851,
3.44255472911916));
#22960=CARTESIAN_POINT('Ctrl Pts',(5.51892784216155,0.270233315828591,3.51242235806964));
#22961=CARTESIAN_POINT('Ctrl Pts',(5.54278576019296,0.470813450024345,3.70151600181885));
#22962=CARTESIAN_POINT('Ctrl Pts',(5.56664367822439,0.556266870991092,3.96359711366712));
#22963=CARTESIAN_POINT('Ctrl Pts',(5.5905015962558,0.505697889589837,4.23457972281303));
#22964=CARTESIAN_POINT('Ctrl Pts',(5.61435951428722,0.331471999260015,4.4482011999181));
#22965=CARTESIAN_POINT('Ctrl Pts',(5.63821743231864,0.0761921759760934,
4.55222527486821));
#22966=CARTESIAN_POINT('Ctrl Pts',(5.66207535035006,-0.197718709731212,
4.52121522783523));
#22967=CARTESIAN_POINT('Ctrl Pts',(5.68593326838148,-0.423281985227643,
4.3627538599096));
#22968=CARTESIAN_POINT('Ctrl Pts',(5.70979118641289,-0.545341285237878,
4.11558929214995));
#22969=CARTESIAN_POINT('Ctrl Pts',(5.73364910444432,-0.534049786451273,
3.84015999362387));
#22970=CARTESIAN_POINT('Ctrl Pts',(5.75750702247573,-0.392168567195948,
3.6038159310769));
#22971=CARTESIAN_POINT('Ctrl Pts',(5.78136494050716,-0.154391451667357,
3.46434966433946));
#22972=CARTESIAN_POINT('Ctrl Pts',(5.80522285853857,0.121138580962943,3.45586449715393));
#22973=CARTESIAN_POINT('Ctrl Pts',(5.82908077656999,0.367046927720705,3.58043527923202));
#22974=CARTESIAN_POINT('Ctrl Pts',(5.85293869460141,0.523202308305842,3.80760107017232));
#22975=CARTESIAN_POINT('Ctrl Pts',(5.87679661263283,0.551420461789987,4.08181362911724));
#22976=CARTESIAN_POINT('Ctrl Pts',(5.90065453066425,0.44480131269862,4.33602054829434));
#22977=CARTESIAN_POINT('Ctrl Pts',(5.92451244869567,0.229416087376931,4.50806125053784));
#22978=CARTESIAN_POINT('Ctrl Pts',(5.94837036672709,-0.042067546589846,
4.55586721297736));
#22979=CARTESIAN_POINT('Ctrl Pts',(5.97222828475851,-0.30326465903273,4.46774835821298));
#22980=CARTESIAN_POINT('Ctrl Pts',(5.99608620278993,-0.490305038147314,
4.26525255699254));
#22981=CARTESIAN_POINT('Ctrl Pts',(6.01994412082133,-0.557452977205748,
3.99789477357902));
#22982=CARTESIAN_POINT('Ctrl Pts',(6.04380203885278,-0.488287539408226,
3.73105273207384));
#22983=CARTESIAN_POINT('Ctrl Pts',(6.06765995688417,-0.299724270968661,
3.52997381710292));
#22984=CARTESIAN_POINT('Ctrl Pts',(6.09151787491561,-0.0378669053578504,
3.44383251805177));
#22985=CARTESIAN_POINT('Ctrl Pts',(6.11537579294702,0.233243627260218,3.49368287747685));
#22986=CARTESIAN_POINT('Ctrl Pts',(6.13923371097844,0.447331678364145,3.6673537262422));
#22987=CARTESIAN_POINT('Ctrl Pts',(6.16309162900986,0.552012406214274,3.92234268746235));
#22988=CARTESIAN_POINT('Ctrl Pts',(6.18694954704127,0.521753629494025,4.19636433484848));
#22989=CARTESIAN_POINT('Ctrl Pts',(6.2108074650727,0.363831507594212,4.42228768590875));
#22990=CARTESIAN_POINT('Ctrl Pts',(6.23466538310411,0.117094415953721,4.54510476979165));
#22991=CARTESIAN_POINT('Ctrl Pts',(6.25852330113554,-0.158561881267111,
4.53433708369694));
#22992=CARTESIAN_POINT('Ctrl Pts',(6.28238121916695,-0.394905399742298,
4.39345989467659));
#22993=CARTESIAN_POINT('Ctrl Pts',(6.30623913719837,-0.535697351746728,
4.1553358869807));
#22994=CARTESIAN_POINT('Ctrl Pts',(6.33009705522979,-0.543633587309765,
3.88114808171798));
#22995=CARTESIAN_POINT('Ctrl Pts',(6.36190761260502,-0.381130543103143,
3.54983775818315));
#22996=CARTESIAN_POINT('Ctrl Pts',(6.40167080932404,0.0904237977681596,
3.37418170676098));
#22997=CARTESIAN_POINT('Ctrl Pts',(6.4493866453869,0.576013642360818,3.73827828410759));
#22998=CARTESIAN_POINT('Ctrl Pts',(6.49710248144972,0.531303907723303,4.34259299019566));
#22999=CARTESIAN_POINT('Ctrl Pts',(6.54481831751257,-0.000617460830772086,
4.63236849138271));
#23000=CARTESIAN_POINT('Ctrl Pts',(6.5925341535754,-0.532336898979176,4.34139325430452));
#23001=CARTESIAN_POINT('Ctrl Pts',(6.64024998963824,-0.575010046738857,
3.73693099107234));
#23002=CARTESIAN_POINT('Ctrl Pts',(6.68796582570108,-0.0897448725589052,
3.37403863313417));
#23003=CARTESIAN_POINT('Ctrl Pts',(6.73568166176391,0.477988548433368,3.58598174571673));
#23004=CARTESIAN_POINT('Ctrl Pts',(6.78339749782676,0.606749053262868,4.17812127049189));
#23005=CARTESIAN_POINT('Ctrl Pts',(6.83111333388958,0.178337754027021,4.60669083891839));
#23006=CARTESIAN_POINT('Ctrl Pts',(6.87882916995244,-0.413851892207341,
4.47812605548031));
#23007=CARTESIAN_POINT('Ctrl Pts',(6.92654500601527,-0.625990718083913,
3.91049119230943));
#23008=CARTESIAN_POINT('Ctrl Pts',(6.97426084207811,-0.263274891453005,
3.42505341469988));
#23009=CARTESIAN_POINT('Ctrl Pts',(7.02197667814094,0.341211513798207,3.46759805477058));
#23010=CARTESIAN_POINT('Ctrl Pts',(7.06969251420378,0.63235750294684,3.99905552874491));
#23011=CARTESIAN_POINT('Ctrl Pts',(7.11740835026662,0.342800202184808,4.53138035934227));
#23012=CARTESIAN_POINT('Ctrl Pts',(7.16512418632946,-0.261555976381552,
4.57573041153878));
#23013=CARTESIAN_POINT('Ctrl Pts',(7.2128400223923,-0.625721183287191,4.0913783776429));
#23014=CARTESIAN_POINT('Ctrl Pts',(7.26055585845514,-0.41527704940159,3.52311216844965));
#23015=CARTESIAN_POINT('Ctrl Pts',(7.30827169451797,0.176522415171576,3.39277939551711));
#23016=CARTESIAN_POINT('Ctrl Pts',(7.35598753058081,0.606218615784068,3.8200666455489));
#23017=CARTESIAN_POINT('Ctrl Pts',(7.40370336664364,0.479214941044062,4.4125894643569));
#23018=CARTESIAN_POINT('Ctrl Pts',(7.4514192027065,-0.0878591916424711,
4.62622502914213));
#23019=CARTESIAN_POINT('Ctrl Pts',(7.49913503876932,-0.574250874682306,
4.26478851416677));
#23020=CARTESIAN_POINT('Ctrl Pts',(7.54685087483217,-0.53329914461431,3.6601926322252));
#23021=CARTESIAN_POINT('Ctrl Pts',(7.594566710895,-0.00261060360317682,
3.36764708477891));
#23022=CARTESIAN_POINT('Ctrl Pts',(7.64228254695784,0.530475294557976,3.65580094934904));
#23023=CARTESIAN_POINT('Ctrl Pts',(7.68999838302067,0.576417567478113,4.26003809833172));
#23024=CARTESIAN_POINT('Ctrl Pts',(7.73771421908353,0.093026718772369,4.62547826040714));
#23025=CARTESIAN_POINT('Ctrl Pts',(7.78543005514634,-0.475791997136335,
4.41653211173522));
#23026=CARTESIAN_POINT('Ctrl Pts',(7.8331458912092,-0.607683601098078,3.82507811568403));
#23027=CARTESIAN_POINT('Ctrl Pts',(7.88086172727203,-0.181530003744534,
3.39425757752065));
#23028=CARTESIAN_POINT('Ctrl Pts',(7.92857756333487,0.411325389238953,3.51969962646458));
#23029=CARTESIAN_POINT('Ctrl Pts',(7.97629339939771,0.626454348233276,4.08620889879763));
#23030=CARTESIAN_POINT('Ctrl Pts',(8.02400923546054,0.266300640003926,4.57355121287022));
#23031=CARTESIAN_POINT('Ctrl Pts',(8.07172507152339,-0.338401043502061,
4.5341926229444));
#23032=CARTESIAN_POINT('Ctrl Pts',(8.11944090758622,-0.632343841791292,
4.00427672775865));
#23033=CARTESIAN_POINT('Ctrl Pts',(8.16715674364906,-0.345595560302635,
3.47043344766624));
#23034=CARTESIAN_POINT('Ctrl Pts',(8.2148725797119,0.258518441882999,3.42289928101069));
#23035=CARTESIAN_POINT('Ctrl Pts',(8.26258841577473,0.625230981070026,3.90532558443901));
#23036=CARTESIAN_POINT('Ctrl Pts',(8.31030425183758,0.417784289925175,4.47469286043008));
#23037=CARTESIAN_POINT('Ctrl Pts',(8.35802008790041,-0.173320143095541,
4.60814237859973));
#23038=CARTESIAN_POINT('Ctrl Pts',(8.40573592396325,-0.605262021838435,
4.18312539302794));
#23039=CARTESIAN_POINT('Ctrl Pts',(8.45345176002609,-0.481382472773795,
3.58994154129225));
#23040=CARTESIAN_POINT('Ctrl Pts',(8.50116759608892,0.0845580080604409,
3.37332068174828));
#23041=CARTESIAN_POINT('Ctrl Pts',(8.54888343215178,0.572847569000584,3.73218908285563));
#23042=CARTESIAN_POINT('Ctrl Pts',(8.59659926821459,0.535082392934658,4.33699236997728));
#23043=CARTESIAN_POINT('Ctrl Pts',(8.64431510427745,0.00594282213592907,
4.6323303784547));
#23044=CARTESIAN_POINT('Ctrl Pts',(8.69203094034027,-0.528654133672296,
4.34698967074364));
#23045=CARTESIAN_POINT('Ctrl Pts',(8.73974677640312,-0.577779864139828,
3.74300300926635));
#23046=CARTESIAN_POINT('Ctrl Pts',(8.78746261246595,-0.0963214550818077,
3.37502063878676));
#23047=CARTESIAN_POINT('Ctrl Pts',(8.8351784485288,0.473590428273928,3.58096643225285));
#23048=CARTESIAN_POINT('Ctrl Pts',(8.88289428459164,0.608596934220305,4.17171719864135));
#23049=CARTESIAN_POINT('Ctrl Pts',(8.93061012065447,0.184719511004659,4.60477741930878));
#23050=CARTESIAN_POINT('Ctrl Pts',(8.97832595671731,-0.408788681441581,
4.48246123012823));
#23051=CARTESIAN_POINT('Ctrl Pts',(9.02604179278014,-0.626899937697651,
3.91709346970068));
#23052=CARTESIAN_POINT('Ctrl Pts',(9.07375762884299,-0.269319335070538,
3.42786005172794));
#23053=CARTESIAN_POINT('Ctrl Pts',(9.12147346490582,0.335581356962483,3.46403155175812));
#23054=CARTESIAN_POINT('Ctrl Pts',(9.16918930096866,0.632312525313962,3.99239112474344));
#23055=CARTESIAN_POINT('Ctrl Pts',(9.21690513703149,0.348381372290835,4.52773804495445));
#23056=CARTESIAN_POINT('Ctrl Pts',(9.26462097309434,-0.255473755443411,
4.5784549981902));
#23057=CARTESIAN_POINT('Ctrl Pts',(9.31233680915717,-0.624723402584967,
4.09796782591368));
#23058=CARTESIAN_POINT('Ctrl Pts',(9.36005264522002,-0.420279936527615,
3.52751529167185));
#23059=CARTESIAN_POINT('Ctrl Pts',(9.40776848128285,0.170113062081096,3.39095273519949));
#23060=CARTESIAN_POINT('Ctrl Pts',(9.45548431734569,0.604288618254829,3.81368765339017));
#23061=CARTESIAN_POINT('Ctrl Pts',(9.50320015340853,0.483536638109595,4.40751606625661));
#23062=CARTESIAN_POINT('Ctrl Pts',(9.55091598947137,-0.0812544769791981,
4.62711620503893));
#23063=CARTESIAN_POINT('Ctrl Pts',(9.5986318255342,-0.571428355597161,4.27082588331087));
#23064=CARTESIAN_POINT('Ctrl Pts',(9.64634766159704,-0.536850782714826,
3.66583198574659));
#23065=CARTESIAN_POINT('Ctrl Pts',(9.69406349765987,-0.0092748755543832,
3.36770971750703));
#23066=CARTESIAN_POINT('Ctrl Pts',(9.74177933372272,0.52681829253995,3.65022934471732));
#23067=CARTESIAN_POINT('Ctrl Pts',(9.78949516978555,0.579126116453474,4.253948746587));
#23068=CARTESIAN_POINT('Ctrl Pts',(9.83721100584839,0.099613516627068,4.62446310696212));
#23069=CARTESIAN_POINT('Ctrl Pts',(9.88492684191123,-0.471375708268938,
4.42152338761395));
#23070=CARTESIAN_POINT('Ctrl Pts',(9.93264267797408,-0.609493367214024,
3.83149225544889));
#23071=CARTESIAN_POINT('Ctrl Pts',(9.9803585140369,-0.187903888785556,3.39620437793004));
#23072=CARTESIAN_POINT('Ctrl Pts',(10.0280743500997,0.406240621987656,3.51539131074786));
#23073=CARTESIAN_POINT('Ctrl Pts',(10.0757901861626,0.627328118774167,4.07960185956908));
#23074=CARTESIAN_POINT('Ctrl Pts',(10.1235060222254,0.27233055140652,4.57071279591595));
#23075=CARTESIAN_POINT('Ctrl Pts',(10.1712218582883,-0.332752351661881,
4.5377293902281));
#23076=CARTESIAN_POINT('Ctrl Pts',(10.2189376943511,-0.632263650146131,
4.01094081146358));
#23077=CARTESIAN_POINT('Ctrl Pts',(10.2666535304139,-0.351157510074434,
3.47410511718603));
#23078=CARTESIAN_POINT('Ctrl Pts',(10.3143693664768,0.252421974751429,3.42020678572945));
#23079=CARTESIAN_POINT('Ctrl Pts',(10.3620852025396,0.624198476151732,3.89874148420283));
#23080=CARTESIAN_POINT('Ctrl Pts',(10.4098010386024,0.422763912373798,4.47026343579529));
#23081=CARTESIAN_POINT('Ctrl Pts',(10.4575168746653,-0.166901257195935,
4.60993523836389));
#23082=CARTESIAN_POINT('Ctrl Pts',(10.5052327107281,-0.603298434176698,
4.18949412648294));
#23083=CARTESIAN_POINT('Ctrl Pts',(10.552948546791,-0.485677376113382,3.5950376425108));
#23084=CARTESIAN_POINT('Ctrl Pts',(10.6006643828538,0.0779486895418537,
3.3724643225678));
#23085=CARTESIAN_POINT('Ctrl Pts',(10.6483802189166,0.569993274196054,3.72616667108832));
#23086=CARTESIAN_POINT('Ctrl Pts',(10.6960960549795,0.538604264682155,4.3313343790158));
#23087=CARTESIAN_POINT('Ctrl Pts',(10.7438118910423,0.0126066714187673,
4.63223262845832));
#23088=CARTESIAN_POINT('Ctrl Pts',(10.7915277271052,-0.524967822187051,
4.35254192703816));
#23089=CARTESIAN_POINT('Ctrl Pts',(10.839243563168,-0.580456287010268,3.74910654946403));
#23090=CARTESIAN_POINT('Ctrl Pts',(10.8869593992308,-0.102902812003948,
3.37607048800905));
#23091=CARTESIAN_POINT('Ctrl Pts',(10.9346752352937,0.469147898628881,3.5759984978049));
#23092=CARTESIAN_POINT('Ctrl Pts',(10.9823910713565,0.610372875182502,4.16529361116822));
#23093=CARTESIAN_POINT('Ctrl Pts',(11.0301069074193,0.191083048662156,4.60279705802663));
#23094=CARTESIAN_POINT('Ctrl Pts',(11.0778227434822,-0.403681281635282,
4.48674269127424));
#23095=CARTESIAN_POINT('Ctrl Pts',(11.125538579545,-0.627738879572117,3.92370502162571));
#23096=CARTESIAN_POINT('Ctrl Pts',(11.1732544156079,-0.275334205393669,
3.43073020456744));
#23097=CARTESIAN_POINT('Ctrl Pts',(11.2209702516707,0.329914106159097,3.46052459999659));
#23098=CARTESIAN_POINT('Ctrl Pts',(11.2686860877335,0.632197217644931,3.98572755614488));
#23099=CARTESIAN_POINT('Ctrl Pts',(11.3164019237964,0.353923896562866,4.52403711709511));
#23100=CARTESIAN_POINT('Ctrl Pts',(11.3641177598592,-0.24936318455202,4.58111533006939));
#23101=CARTESIAN_POINT('Ctrl Pts',(11.411833595922,-0.623656216347001,4.10454639383227));
#23102=CARTESIAN_POINT('Ctrl Pts',(11.4595494319849,-0.425236148486169,
3.53197089548594));
#23103=CARTESIAN_POINT('Ctrl Pts',(11.5072652680477,0.163684817628688,3.3891937253683));
#23104=CARTESIAN_POINT('Ctrl Pts',(11.5549811041106,0.602291497100466,3.80732935570755));
#23105=CARTESIAN_POINT('Ctrl Pts',(11.6026969401734,0.487804627338989,4.40239740331947));
#23106=CARTESIAN_POINT('Ctrl Pts',(11.6504127762363,-0.0746407375468588,
4.62793772378323));
#23107=CARTESIAN_POINT('Ctrl Pts',(11.6981286122991,-0.568542364648052,
4.276833170433));
#23108=CARTESIAN_POINT('Ctrl Pts',(11.7458444483619,-0.540342790144192,
3.67150845704832));
#23109=CARTESIAN_POINT('Ctrl Pts',(11.7935602844247,-0.0159381172083995,
3.36784258204823));
#23110=CARTESIAN_POINT('Ctrl Pts',(11.8412761204876,0.523102773999324,3.64469659094542));
#23111=CARTESIAN_POINT('Ctrl Pts',(11.8889919565504,0.581770338872691,4.24783118742311));
#23112=CARTESIAN_POINT('Ctrl Pts',(11.9367077926133,0.106189249871976,4.62337859111715));
#23113=CARTESIAN_POINT('Ctrl Pts',(11.9844236286761,-0.466907061217805,
4.4264678426758));
#23114=CARTESIAN_POINT('Ctrl Pts',(12.0321394647389,-0.611235433702689,
3.83792511225401));
#23115=CARTESIAN_POINT('Ctrl Pts',(12.0798553008018,-0.19425690235234,3.39821824509208));
#23116=CARTESIAN_POINT('Ctrl Pts',(12.1275711368646,0.401110731454808,3.51113682306459));
#23117=CARTESIAN_POINT('Ctrl Pts',(12.1752869729275,0.628132208685083,4.07298597854376));
#23118=CARTESIAN_POINT('Ctrl Pts',(12.2230028089903,0.27833021362349,4.56781098689255));
#23119=CARTESIAN_POINT('Ctrl Pts',(12.2707186450531,-0.327066699269377,
4.54120642908287));
#23120=CARTESIAN_POINT('Ctrl Pts',(12.3184344811159,-0.632113229655128,
4.01760367991507));
#23121=CARTESIAN_POINT('Ctrl Pts',(12.3661503171788,-0.356680454936339,
3.47783520061383));
#23122=CARTESIAN_POINT('Ctrl Pts',(12.4138661532416,0.246297469784735,3.4175786911271));
#23123=CARTESIAN_POINT('Ctrl Pts',(12.4615819893045,0.623096638228782,3.89216863128209));
#23124=CARTESIAN_POINT('Ctrl Pts',(12.5092978253673,0.427696576213203,4.46578177652963));
#23125=CARTESIAN_POINT('Ctrl Pts',(12.5570136614302,-0.16046383269669,4.61166034941614));
#23126=CARTESIAN_POINT('Ctrl Pts',(12.604729497493,-0.601267834987779,4.1958418118296));
#23127=CARTESIAN_POINT('Ctrl Pts',(12.6524453335558,-0.489918332714758,
3.60017872502631));
#23128=CARTESIAN_POINT('Ctrl Pts',(12.7001611696187,0.0713307128527425,
3.37167766707246));
#23129=CARTESIAN_POINT('Ctrl Pts',(12.7478770056815,0.56707566724347,3.72017467542775));
#23130=CARTESIAN_POINT('Ctrl Pts',(12.7955928417444,0.542066310823814,4.32563958500381));
#23131=CARTESIAN_POINT('Ctrl Pts',(12.8433086778072,0.0192691204123526,
4.63206465306178));
#23132=CARTESIAN_POINT('Ctrl Pts',(12.89102451387,-0.521223199767296,4.35805502464836));
#23133=CARTESIAN_POINT('Ctrl Pts',(12.9387403499329,-0.583068235550835,
3.7552379577156));
#23134=CARTESIAN_POINT('Ctrl Pts',(12.9864561859957,-0.109472738970043,
3.37718964036075));
#23135=CARTESIAN_POINT('Ctrl Pts',(13.0341720220585,0.464653258261548,3.57107765943178));
#23136=CARTESIAN_POINT('Ctrl Pts',(13.0818878581214,0.612081018822183,4.15885166366515));
#23137=CARTESIAN_POINT('Ctrl Pts',(13.1296036941842,0.197425361721354,4.6007497409078));
#23138=CARTESIAN_POINT('Ctrl Pts',(13.177319530247,-0.398529042827853,4.49097008735187));
#23139=CARTESIAN_POINT('Ctrl Pts',(13.2250353663099,-0.628508095190705,
3.93032504803489));
#23140=CARTESIAN_POINT('Ctrl Pts',(13.2727512023727,-0.281318492899819,
3.4336635891944));
#23141=CARTESIAN_POINT('Ctrl Pts',(13.3204670384356,0.324210210062374,3.45707757060249));
#23142=CARTESIAN_POINT('Ctrl Pts',(13.3681828744984,0.632011688508986,3.97906557286167));
#23143=CARTESIAN_POINT('Ctrl Pts',(13.4158987105612,0.359427108647973,4.52027798167956));
#23144=CARTESIAN_POINT('Ctrl Pts',(13.4636145466241,-0.243224915581421,
4.58371111441534));
#23145=CARTESIAN_POINT('Ctrl Pts',(13.5113303826869,-0.622519757336015,
4.11111334923356));
#23146=CARTESIAN_POINT('Ctrl Pts',(13.5590462187498,-0.430145127231255,
3.53647848575196));
#23147=CARTESIAN_POINT('Ctrl Pts',(13.6067620548126,0.157238391843492,3.38750256099959));
#23148=CARTESIAN_POINT('Ctrl Pts',(13.6544778908755,0.600227476264717,3.8009924589658));
#23149=CARTESIAN_POINT('Ctrl Pts',(13.7021937269383,0.492018433545193,4.39723404398833));
#23150=CARTESIAN_POINT('Ctrl Pts',(13.7499095630011,-0.0680187073756014,
4.62868949418496));
#23151=CARTESIAN_POINT('Ctrl Pts',(13.797625399064,-0.565593222711038,4.28280970824024));
#23152=CARTESIAN_POINT('Ctrl Pts',(13.8453412351268,-0.543774778860562,
3.67722141563181));
#23153=CARTESIAN_POINT('Ctrl Pts',(13.8930570711896,-0.0225995885319848,
3.36804566363559));
#23154=CARTESIAN_POINT('Ctrl Pts',(13.9407729072525,0.519329151684885,3.63920330259016));
#23155=CARTESIAN_POINT('Ctrl Pts',(13.9884887433153,0.584349941003394,4.24168610034696));
#23156=CARTESIAN_POINT('Ctrl Pts',(14.0362045793781,0.112753188118911,4.62222483333648));
#23157=CARTESIAN_POINT('Ctrl Pts',(14.083920415441,-0.462386552345973,4.43136492771341));
#23158=CARTESIAN_POINT('Ctrl Pts',(14.1316362515038,-0.612909607059929,
3.84437597156854));
#23159=CARTESIAN_POINT('Ctrl Pts',(14.1793520875667,-0.200588338784227,
3.40029895531576));
#23160=CARTESIAN_POINT('Ctrl Pts',(14.2270679236295,0.395936287445344,3.50693663598317));
#23161=CARTESIAN_POINT('Ctrl Pts',(14.2747837596923,0.628866528650988,4.06636199058228));
#23162=CARTESIAN_POINT('Ctrl Pts',(14.3224995957552,0.284298960241116,4.5648461081192));
#23163=CARTESIAN_POINT('Ctrl Pts',(14.370215431818,-0.321344717859966,4.54462335329573));
#23164=CARTESIAN_POINT('Ctrl Pts',(14.4179312678809,-0.631892597026201,
4.02426459303334));
#23165=CARTESIAN_POINT('Ctrl Pts',(14.4656471039437,-0.362163781425906,
3.48162328362967));
#23166=CARTESIAN_POINT('Ctrl Pts',(14.5133629400065,0.240145607263868,3.41501528911991));
#23167=CARTESIAN_POINT('Ctrl Pts',(14.5610787760693,0.6219255896881,3.8856077557581));
#23168=CARTESIAN_POINT('Ctrl Pts',(14.6087946121322,0.432581733546503,4.46124838043455));
#23169=CARTESIAN_POINT('Ctrl Pts',(14.656510448195,-0.154008584636381,4.61331752013935));
#23170=CARTESIAN_POINT('Ctrl Pts',(14.7042262842579,-0.599170449821005,
4.20216774399712));
#23171=CARTESIAN_POINT('Ctrl Pts',(14.7519421203207,-0.494104871512583,
3.60536421779174));
#23172=CARTESIAN_POINT('Ctrl Pts',(14.7996579563836,0.0647048130865326,
3.37096080264023));
#23173=CARTESIAN_POINT('Ctrl Pts',(14.8473737924464,0.564095072216763,3.71421376143635));
#23174=CARTESIAN_POINT('Ctrl Pts',(14.8950896285093,0.545468146811986,4.319908620492));
#23175=CARTESIAN_POINT('Ctrl Pts',(14.942805464572,0.0259294290834894,4.63182647092298));
#23176=CARTESIAN_POINT('Ctrl Pts',(14.9905213006349,-0.517420682347921,
4.36352835120552));
#23177=CARTESIAN_POINT('Ctrl Pts',(15.0382371366977,-0.585615419638682,
3.76139655297334));
#23178=CARTESIAN_POINT('Ctrl Pts',(15.0859529727606,-0.116030506223773,
3.3783779715317));
#23179=CARTESIAN_POINT('Ctrl Pts',(15.1336688088234,0.460107006415252,3.56620446371685));
#23180=CARTESIAN_POINT('Ctrl Pts',(15.1813846448862,0.613721175406852,4.15239207167311));
#23181=CARTESIAN_POINT('Ctrl Pts',(15.2291004809491,0.203745745708236,4.59863569535852));
#23182=CARTESIAN_POINT('Ctrl Pts',(15.2768163170119,-0.393332537305518,
4.49514294880206));
#23183=CARTESIAN_POINT('Ctrl Pts',(15.3245321530748,-0.629207499112597,
3.93695281360709));
#23184=CARTESIAN_POINT('Ctrl Pts',(15.3722479891376,-0.287271532882751,
3.43665987978239));
#23185=CARTESIAN_POINT('Ctrl Pts',(15.4199638252004,0.318470302234025,3.45369084645546));
#23186=CARTESIAN_POINT('Ctrl Pts',(15.4676796612633,0.631755958513824,3.97240591487529));
#23187=CARTESIAN_POINT('Ctrl Pts',(15.5153954973261,0.364890397275464,4.51646105625472));
#23188=CARTESIAN_POINT('Ctrl Pts',(15.563111333389,-0.237059630341402,4.58624206290064));
#23189=CARTESIAN_POINT('Ctrl Pts',(15.6108271694518,-0.621314151784485,
4.11766796269128));
#23190=CARTESIAN_POINT('Ctrl Pts',(15.6585430055147,-0.435006327496808,
3.54103756178819));
#23191=CARTESIAN_POINT('Ctrl Pts',(15.7062588415774,0.150774500763906,3.38587942993986));
#23192=CARTESIAN_POINT('Ctrl Pts',(15.7539746776403,0.598096785009218,3.79467766703735));
#23193=CARTESIAN_POINT('Ctrl Pts',(15.8016905137032,0.496177588678611,4.39202656178461));
#23194=CARTESIAN_POINT('Ctrl Pts',(15.849406349766,-0.0613891220090978,
4.62937143274106));
#23195=CARTESIAN_POINT('Ctrl Pts',(15.8971221858288,-0.562581257362808,
4.28875483288714));
#23196=CARTESIAN_POINT('Ctrl Pts',(15.9448380218917,-0.547146367654922,
3.68297022692873));
#23197=CARTESIAN_POINT('Ctrl Pts',(15.9925538579545,-0.0292585496004989,
3.36831893971177));
#23198=CARTESIAN_POINT('Ctrl Pts',(16.0402696940173,0.515497844752703,3.63375008981994));
#23199=CARTESIAN_POINT('Ctrl Pts',(16.0879855300802,0.586864636315616,4.23551416792571));
#23200=CARTESIAN_POINT('Ctrl Pts',(16.135701366143,0.119304602276749,4.62100196177401));
#23201=CARTESIAN_POINT('Ctrl Pts',(16.1834172022059,-0.457814683770117,
4.43621409878185));
#23202=CARTESIAN_POINT('Ctrl Pts',(16.2311330382687,-0.614515701326505,
3.85084411686165));
#23203=CARTESIAN_POINT('Ctrl Pts',(16.2788488743316,-0.206897494815317,
3.40244627748567));
#23204=CARTESIAN_POINT('Ctrl Pts',(16.3265647103943,0.390717864711932,3.50279121604045));
#23205=CARTESIAN_POINT('Ctrl Pts',(16.3742805464572,0.629530997107116,4.05973063144581));
#23206=CARTESIAN_POINT('Ctrl Pts',(16.42199638252,0.290236128279341,4.56181848892059));
#23207=CARTESIAN_POINT('Ctrl Pts',(16.4697122185829,-0.315587043004215,
4.54797978333095));
#23208=CARTESIAN_POINT('Ctrl Pts',(16.5174280546457,-0.631601776766168,
4.03092281095576));
#23209=CARTESIAN_POINT('Ctrl Pts',(16.5651438907086,-0.367606880481235,
3.48546894547127));
#23210=CARTESIAN_POINT('Ctrl Pts',(16.6128597267714,0.233967070508539,3.41251686443844));
#23211=CARTESIAN_POINT('Ctrl Pts',(16.6605755628343,0.620685460604191,3.87905958638177));
#23212=CARTESIAN_POINT('Ctrl Pts',(16.7082913988971,0.437418841753611,4.45666375105816));
#23213=CARTESIAN_POINT('Ctrl Pts',(16.7560072349599,-0.147536230033309,
4.61490656646286));
#23214=CARTESIAN_POINT('Ctrl Pts',(16.8037230710227,-0.597006511643959,
4.20847122033102));
#23215=CARTESIAN_POINT('Ctrl Pts',(16.8514389070856,-0.498236527486006,
3.61059354482716));
#23216=CARTESIAN_POINT('Ctrl Pts',(16.8991547431484,0.058071726216741,3.37031380889701));
#23217=CARTESIAN_POINT('Ctrl Pts',(16.9468705792113,0.561051820186282,3.70828459122417));
#23218=CARTESIAN_POINT('Ctrl Pts',(16.9945864152741,0.548809394786867,4.31414212204871));
#23219=CARTESIAN_POINT('Ctrl Pts',(17.0423022513369,0.0325868576366809,
4.63151810849805));
#23220=CARTESIAN_POINT('Ctrl Pts',(17.0900180873998,-0.513560692294518,
4.3689612987585));
#23221=CARTESIAN_POINT('Ctrl Pts',(17.1377339234626,-0.588097556344686,
3.76758165116972));
#23222=CARTESIAN_POINT('Ctrl Pts',(17.1854497595255,-0.122575385359494,
3.37963534952775));
#23223=CARTESIAN_POINT('Ctrl Pts',(17.2331655955883,0.455509648066065,3.56137945195155));
#23224=CARTESIAN_POINT('Ctrl Pts',(17.2808814316511,0.615293162755707,4.14591555269289));
#23225=CARTESIAN_POINT('Ctrl Pts',(17.328597267714,0.210043498584534,4.59645515619697));
#23226=CARTESIAN_POINT('Ctrl Pts',(17.3763131037768,-0.388092342271454,
4.49926081212312));
#23227=CARTESIAN_POINT('Ctrl Pts',(17.4240289398397,-0.629837013651323,
3.94358758216158));
#23228=CARTESIAN_POINT('Ctrl Pts',(17.4717447759025,-0.293192664107019,
3.43971874351766));
#23229=CARTESIAN_POINT('Ctrl Pts',(17.5194606119653,0.312695020235776,3.45036480373676));
#23230=CARTESIAN_POINT('Ctrl Pts',(17.5671764480282,0.631430056064715,3.96574932190893));
#23231=CARTESIAN_POINT('Ctrl Pts',(17.614892284091,0.370313155609181,4.51258676478657));
#23232=CARTESIAN_POINT('Ctrl Pts',(17.6626081201539,-0.230868013642575,
4.58870789439952));
#23233=CARTESIAN_POINT('Ctrl Pts',(17.7103239562166,-0.620039533605355,
4.12420950615009));
#23234=CARTESIAN_POINT('Ctrl Pts',(17.7580397922796,-0.43981920932378,3.54564761719411));
#23235=CARTESIAN_POINT('Ctrl Pts',(17.8057556283423,0.144293862368219,3.38432451247882));
#23236=CARTESIAN_POINT('Ctrl Pts',(17.8534714644052,0.595899660001039,3.78838568133928));
#23237=CARTESIAN_POINT('Ctrl Pts',(17.901187300468,0.500281630760053,4.38677553513073));
#23238=CARTESIAN_POINT('Ctrl Pts',(17.9489031365309,-0.0547527178302441,
4.62998346370502));
#23239=CARTESIAN_POINT('Ctrl Pts',(17.9966189725937,-0.559506803158163,
4.29466788401745));
#23240=CARTESIAN_POINT('Ctrl Pts',(18.0443348086565,-0.550457182027191,
3.68875425238845));
#23241=CARTESIAN_POINT('Ctrl Pts',(18.0920506447194,-0.0359142607682062,
3.36866237992255));
#23242=CARTESIAN_POINT('Ctrl Pts',(18.1397664807822,0.511609278766163,3.62833755835171));
#23243=CARTESIAN_POINT('Ctrl Pts',(18.187482316845,0.589314145488933,4.22931607570827));
#23244=CARTESIAN_POINT('Ctrl Pts',(18.2351981529079,0.12584276464555,4.61971011226051));
#23245=CARTESIAN_POINT('Ctrl Pts',(18.2829139889707,-0.453191963311679,
4.44101481725822));
#23246=CARTESIAN_POINT('Ctrl Pts',(18.3306298250336,-0.616053538105107,
3.85732882968247));
#23247=CARTESIAN_POINT('Ctrl Pts',(18.3783456610964,-0.213183669654489,
3.40465997308746));
#23248=CARTESIAN_POINT('Ctrl Pts',(18.4260614971592,0.385456042892229,3.49870102369));
#23249=CARTESIAN_POINT('Ctrl Pts',(18.4737773332221,0.630125540247444,4.05309263771424));
#23250=CARTESIAN_POINT('Ctrl Pts',(18.5214931692849,0.296141058265729,4.55872846559028));
#23251=CARTESIAN_POINT('Ctrl Pts',(18.5692090053478,-0.309794314237323,
4.55127534637221));
#23252=CARTESIAN_POINT('Ctrl Pts',(18.6169248414106,-0.631240801177943,
4.0375775941191));
#23253=CARTESIAN_POINT('Ctrl Pts',(18.6646406774734,-0.373009147508776,
3.4893717589807));
#23254=CARTESIAN_POINT('Ctrl Pts',(18.7123565135363,0.227762545801372,3.41008369459593));
#23255=CARTESIAN_POINT('Ctrl Pts',(18.7600723495991,0.619376388724522,3.87252485049244));
#23256=CARTESIAN_POINT('Ctrl Pts',(18.8077881856619,0.442207363551868,4.45202839763978));
#23257=CARTESIAN_POINT('Ctrl Pts',(18.8555040217248,-0.141047487806633,
4.61642731188217));
#23258=CARTESIAN_POINT('Ctrl Pts',(18.9032198577876,-0.594776260815313,
4.21475154067248));
#23259=CARTESIAN_POINT('Ctrl Pts',(18.9509356938505,-0.502312841712761,
3.615866125281));
#23260=CARTESIAN_POINT('Ctrl Pts',(18.9986515299133,0.0514321890198641,
3.36973675771293));
#23261=CARTESIAN_POINT('Ctrl Pts',(19.0463673659762,0.557946249173174,3.70238782336559));
#23262=CARTESIAN_POINT('Ctrl Pts',(19.0940832020389,0.552089683635207,4.30834073020757));
#23263=CARTESIAN_POINT('Ctrl Pts',(19.1417990381018,0.0392406665648073,
4.63113960000379));
#23264=CARTESIAN_POINT('Ctrl Pts',(19.1895148741646,-0.509643658296843,
4.3743532639067));
#23265=CARTESIAN_POINT('Ctrl Pts',(19.2372307102275,-0.590514370077448,
3.77379256516987));
#23266=CARTESIAN_POINT('Ctrl Pts',(19.2849465462903,-0.129106649190522,
3.38096163491845));
#23267=CARTESIAN_POINT('Ctrl Pts',(19.3326623823532,0.450861693465423,3.55660315963506));
#23268=CARTESIAN_POINT('Ctrl Pts',(19.380378218416,0.616796807017627,4.1394228269368));
#23269=CARTESIAN_POINT('Ctrl Pts',(19.4280940544789,0.216317919394901,4.59420836405745));
#23270=CARTESIAN_POINT('Ctrl Pts',(19.4758098905416,-0.382809037079938,
4.50332322288615));
#23271=CARTESIAN_POINT('Ctrl Pts',(19.5235257266046,-0.630396573984801,
3.95022861114352));
#23272=CARTESIAN_POINT('Ctrl Pts',(19.5712415626673,-0.299081219248977,
3.44283985120298));
#23273=CARTESIAN_POINT('Ctrl Pts',(19.6189573987302,0.306884987370396,3.44709979193512));
#23274=CARTESIAN_POINT('Ctrl Pts',(19.666673234793,0.631034051704256,3.95909657101937));
#23275=CARTESIAN_POINT('Ctrl Pts',(19.7143890708559,0.375694716468479,4.50865546647685));
#23276=CARTESIAN_POINT('Ctrl Pts',(19.7621049069187,-0.224650630777236,
4.59110846933868));
#23277=CARTESIAN_POINT('Ctrl Pts',(19.8098207429815,-0.618696275574682,
4.13073699938377));
#23278=CARTESIAN_POINT('Ctrl Pts',(19.8575365790444,-0.44458280157215,3.55030861879767));
#23279=CARTESIAN_POINT('Ctrl Pts',(19.9052524151072,0.13779637220375,3.3828370770856));
#23280=CARTESIAN_POINT('Ctrl Pts',(19.9529682511701,0.593637901716091,3.7821189081517));
#23281=CARTESIAN_POINT('Ctrl Pts',(20.0006840872329,0.504327165075627,4.38147832337345));
#23282=CARTESIAN_POINT('Ctrl Pts',(20.0483999232957,-0.0481046828163007,
4.63053160650705));
#23283=CARTESIAN_POINT('Ctrl Pts',(20.0961157593586,-0.556380679578279,
4.30053671048834));
#23284=CARTESIAN_POINT('Ctrl Pts',(20.1438315954214,-0.553687069357429,
3.69459455385474));
#23285=CARTESIAN_POINT('Ctrl Pts',(20.1915474314843,-0.0426033430871586,
3.36903495876776));
#23286=CARTESIAN_POINT('Ctrl Pts',(20.2392632675471,0.507734449822709,3.62304374442814));
#23287=CARTESIAN_POINT('Ctrl Pts',(20.2869791036099,0.591564791291533,4.22294595084339));
#23288=CARTESIAN_POINT('Ctrl Pts',(20.3346949396728,0.132620199007312,4.618629012875));
#23289=CARTESIAN_POINT('Ctrl Pts',(20.3824107757356,-0.449008129734859,
4.44521533979349));
#23290=CARTESIAN_POINT('Ctrl Pts',(20.4221739724547,-0.588594799935545,
3.96175478680276));
#23291=CARTESIAN_POINT('Ctrl Pts',(20.4539845298298,-0.419131055782338,
3.63395025773895));
#23292=CARTESIAN_POINT('Ctrl Pts',(20.4778424478613,-0.194099195253748,
3.47709810398663));
#23293=CARTESIAN_POINT('Ctrl Pts',(20.5017003658927,0.0810471032980313,
3.44846366347126));
#23294=CARTESIAN_POINT('Ctrl Pts',(20.5255582839241,0.334940048200093,3.55449674151986));
#23295=CARTESIAN_POINT('Ctrl Pts',(20.5494162019556,0.507694843328107,3.76957374638464));
#23296=CARTESIAN_POINT('Ctrl Pts',(20.5732741199869,0.555899439471162,4.04093981905292));
#23297=CARTESIAN_POINT('Ctrl Pts',(20.5971320380184,0.468386015874758,4.30232489481291));
#23298=CARTESIAN_POINT('Ctrl Pts',(20.6209899560498,0.266225827016684,4.48976745893774));
#23299=CARTESIAN_POINT('Ctrl Pts',(20.6448478740812,-0.000973650874560818,
4.55745692740964));
#23300=CARTESIAN_POINT('Ctrl Pts',(20.6687057921126,-0.267966914960919,
4.48882854939535));
#23301=CARTESIAN_POINT('Ctrl Pts',(20.6925637101441,-0.469418090387657,
4.30067062862012));
#23302=CARTESIAN_POINT('Ctrl Pts',(20.7164216281755,-0.556092695039732,
4.03898930289119));
#23303=CARTESIAN_POINT('Ctrl Pts',(20.7402795462069,-0.506782753954552,
3.7677746905255));
#23304=CARTESIAN_POINT('Ctrl Pts',(20.7641374642383,-0.333553132261349,
3.55334514249538));
#23305=CARTESIAN_POINT('Ctrl Pts',(20.7879953822697,-0.0787593560922578,
3.44813505886707));
#23306=CARTESIAN_POINT('Ctrl Pts',(20.8118533003012,0.19529252477751,3.47787088781106));
#23307=CARTESIAN_POINT('Ctrl Pts',(20.8357112183325,0.421590436108717,3.63528155911584));
#23308=CARTESIAN_POINT('Ctrl Pts',(20.859569136364,0.544797804677434,3.8818757964511));
#23309=CARTESIAN_POINT('Ctrl Pts',(20.8834270543954,0.534787374467886,4.15735463375504));
#23310=CARTESIAN_POINT('Ctrl Pts',(20.9072849724269,0.394006808563119,4.39435596913946));
#23311=CARTESIAN_POINT('Ctrl Pts',(20.9311428904582,0.156880874733563,4.53492653211281));
#23312=CARTESIAN_POINT('Ctrl Pts',(20.9550008084897,-0.118606721834374,
4.54469298471526));
#23313=CARTESIAN_POINT('Ctrl Pts',(20.9788587265211,-0.365091735913813,
4.42126716656144));
#23314=CARTESIAN_POINT('Ctrl Pts',(21.0027166445525,-0.522301880015273,
4.19483005048941));
#23315=CARTESIAN_POINT('Ctrl Pts',(21.0265745625839,-0.55179498493052,3.92075168033001));
#23316=CARTESIAN_POINT('Ctrl Pts',(21.0504324806153,-0.446359186657349,
3.66605168284066));
#23317=CARTESIAN_POINT('Ctrl Pts',(21.0742903986468,-0.231776408019839,
3.49301114555638));
#23318=CARTESIAN_POINT('Ctrl Pts',(21.0981483166782,0.0394820154987394,
3.44394319323497));
#23319=CARTESIAN_POINT('Ctrl Pts',(21.1220062347096,0.301086010940692,3.5308462768762));
#23320=CARTESIAN_POINT('Ctrl Pts',(21.145864152741,0.489066275193333,3.73247022529863));
#23321=CARTESIAN_POINT('Ctrl Pts',(21.1697220707724,0.557456513314207,3.9995124910074));
#23322=CARTESIAN_POINT('Ctrl Pts',(21.1935799888039,0.489533449092281,4.26667396594056));
#23323=CARTESIAN_POINT('Ctrl Pts',(21.2174379068352,0.30190612195814,4.46862639215028));
#23324=CARTESIAN_POINT('Ctrl Pts',(21.2412958248667,0.0404545242400231,
4.55598690035157));
#23325=CARTESIAN_POINT('Ctrl Pts',(21.2651537428981,-0.230889306609896,
4.50739346663836));
#23326=CARTESIAN_POINT('Ctrl Pts',(21.2890116609295,-0.445774412697373,
4.33472850921124));
#23327=CARTESIAN_POINT('Ctrl Pts',(21.312869578961,-0.551655532228011,4.08021331346062));
#23328=CARTESIAN_POINT('Ctrl Pts',(21.3367274969923,-0.522641847334507,
3.80608377760199));
#23329=CARTESIAN_POINT('Ctrl Pts',(21.3605854150238,-0.365827994289322,
3.57937204029158));
#23330=CARTESIAN_POINT('Ctrl Pts',(21.3844433330552,-0.119559231686077,
3.45551529680541));
#23331=CARTESIAN_POINT('Ctrl Pts',(21.4083012510867,0.155945019792583,3.46479989471587));
#23332=CARTESIAN_POINT('Ctrl Pts',(21.432159169118,0.393316466074861,3.60495549692644));
#23333=CARTESIAN_POINT('Ctrl Pts',(21.4560170871495,0.534511322676435,3.84171024093472));
#23334=CARTESIAN_POINT('Ctrl Pts',(21.4798750051809,0.545003601087511,4.11717114276091));
#23335=CARTESIAN_POINT('Ctrl Pts',(21.5037329232123,0.422227653432673,4.36398050850424));
#23336=CARTESIAN_POINT('Ctrl Pts',(21.5275908412437,0.196205543263173,4.52178672528827));
#23337=CARTESIAN_POINT('Ctrl Pts',(21.5514487592751,-0.0777941667658609,
4.5520018745543));
#23338=CARTESIAN_POINT('Ctrl Pts',(21.5753066773066,-0.332771083950078,
4.44723752926263));
#23339=CARTESIAN_POINT('Ctrl Pts',(21.5991645953379,-0.506376406606172,
4.23311142556056));
#23340=CARTESIAN_POINT('Ctrl Pts',(21.6230225133694,-0.556158904430687,
3.96198322848119));
#23341=CARTESIAN_POINT('Ctrl Pts',(21.6468804314008,-0.469945400657515,
3.70015116759423));
#23342=CARTESIAN_POINT('Ctrl Pts',(21.6707383494323,-0.268817445367881,
3.51164031394868));
#23343=CARTESIAN_POINT('Ctrl Pts',(21.6945962674636,-0.00195630224560004,
3.44254670619344));
#23344=CARTESIAN_POINT('Ctrl Pts',(21.7184541854951,0.26538321006433,3.50976561349676));
#23345=CARTESIAN_POINT('Ctrl Pts',(21.7423121035264,0.467829298620023,3.6968601820167));
#23346=CARTESIAN_POINT('Ctrl Pts',(21.766170021558,0.555878380248887,3.95808069339639));
#23347=CARTESIAN_POINT('Ctrl Pts',(21.7900279395893,0.508000056083844,4.22955161709966));
#23348=CARTESIAN_POINT('Ctrl Pts',(21.8138858576208,0.335901880562604,4.44489091756156));
#23349=CARTESIAN_POINT('Ctrl Pts',(21.8377437756521,0.0816665454602928,
4.55144227009437));
#23350=CARTESIAN_POINT('Ctrl Pts',(21.8616016936836,-0.192538484559094,
4.52315096660328));
#23351=CARTESIAN_POINT('Ctrl Pts',(21.885459611715,-0.419662610460766,4.36693500143146));
#23352=CARTESIAN_POINT('Ctrl Pts',(21.9093175297464,-0.544167796724789,
4.12099343330092));
#23353=CARTESIAN_POINT('Ctrl Pts',(21.9331754477779,-0.535609133856441,
3.84546567493331));
#23354=CARTESIAN_POINT('Ctrl Pts',(21.9570333658092,-0.396079448060293,
3.60772576847503));
#23355=CARTESIAN_POINT('Ctrl Pts',(21.9808912838407,-0.159697548225882,
3.46590759696012));
#23356=CARTESIAN_POINT('Ctrl Pts',(22.0047492018721,0.115734752223676,3.45468956637345));
#23357=CARTESIAN_POINT('Ctrl Pts',(22.0286071199035,0.362866753203085,3.5768147907664));
#23358=CARTESIAN_POINT('Ctrl Pts',(22.0524650379349,0.521267948732644,3.80242032615069));
#23359=CARTESIAN_POINT('Ctrl Pts',(22.0763229559664,0.552204931742854,4.07633947375325));
#23360=CARTESIAN_POINT('Ctrl Pts',(22.1001808739978,0.448112767182329,4.33159154057792));
#23361=CARTESIAN_POINT('Ctrl Pts',(22.1240387920292,0.23444482469764,4.5057604433585));
#23362=CARTESIAN_POINT('Ctrl Pts',(22.1478967100606,-0.0365512635718279,
4.55625714110116));
#23363=CARTESIAN_POINT('Ctrl Pts',(22.171754628092,-0.298609572266455,4.47073381570218));
#23364=CARTESIAN_POINT('Ctrl Pts',(22.1956125461234,-0.487649706571227,
4.2701032498363));
#23365=CARTESIAN_POINT('Ctrl Pts',(22.2194704641549,-0.557446204325542,
4.00342508191314));
#23366=CARTESIAN_POINT('Ctrl Pts',(22.2433283821863,-0.490931920559466,
3.73590938817905));
#23367=CARTESIAN_POINT('Ctrl Pts',(22.2671863002177,-0.304371409562025,
3.53297104269219));
#23368=CARTESIAN_POINT('Ctrl Pts',(22.2910442182491,-0.0433837978980346,
3.44423399893113));
#23369=CARTESIAN_POINT('Ctrl Pts',(22.3149021362806,0.228212333880327,3.49139688109763));
#23370=CARTESIAN_POINT('Ctrl Pts',(22.3387600543119,0.444004334066149,3.66292708008725));
#23371=CARTESIAN_POINT('Ctrl Pts',(22.3626179723434,0.551225179343846,3.91688078933633));
#23372=CARTESIAN_POINT('Ctrl Pts',(22.3864758903748,0.523656454698273,4.19115941035881));
#23373=CARTESIAN_POINT('Ctrl Pts',(22.4103338084062,0.368039459933637,4.41869434725418));
#23374=CARTESIAN_POINT('Ctrl Pts',(22.4341917264376,0.122426797365049,4.54384711353805));
#23375=CARTESIAN_POINT('Ctrl Pts',(22.458049644469,-0.153122562087755,4.53601444212637));
#23376=CARTESIAN_POINT('Ctrl Pts',(22.4819075625005,-0.391229265084309,
4.39711164706476));
#23377=CARTESIAN_POINT('Ctrl Pts',(22.5057654805319,-0.533669791868601,
4.16110422172694));
#23378=CARTESIAN_POINT('Ctrl Pts',(22.5296233985633,-0.545613449745194,
3.88570245498666));
#23379=CARTESIAN_POINT('Ctrl Pts',(22.5534813165947,-0.424139885198736,
3.63824949626794));
#23380=CARTESIAN_POINT('Ctrl Pts',(22.5773392346261,-0.198952323217499,
3.47925449370713));
#23381=CARTESIAN_POINT('Ctrl Pts',(22.6011971526576,0.0748840438856019,
3.44759575567767));
#23382=CARTESIAN_POINT('Ctrl Pts',(22.625055070689,0.330410085854462,3.55101527375816));
#23383=CARTESIAN_POINT('Ctrl Pts',(22.6489129887204,0.505140231362423,3.7642230866287));
#23384=CARTESIAN_POINT('Ctrl Pts',(22.6727709067518,0.556352908954721,4.03508610068096));
#23385=CARTESIAN_POINT('Ctrl Pts',(22.6966288247833,0.471516332128332,4.29736710820476));
#23386=CARTESIAN_POINT('Ctrl Pts',(22.7204867428146,0.27139215166714,4.48693847894857));
#23387=CARTESIAN_POINT('Ctrl Pts',(22.7443446608461,0.00488440565515616,
4.55743119390072));
#23388=CARTESIAN_POINT('Ctrl Pts',(22.7682025788775,-0.262778018495442,
4.49163382183027));
#23389=CARTESIAN_POINT('Ctrl Pts',(22.7920604969089,-0.466262514422727,
4.30558517247789));
#23390=CARTESIAN_POINT('Ctrl Pts',(22.8079657755965,-0.525793678117208,
4.1317859159904));
#23391=CARTESIAN_POINT('Ctrl Pts',(22.8159184149403,-0.532958495437544,
4.04301651477895));
#23392=CARTESIAN_POINT('Ctrl Pts',(3.98408158505965,-0.251304309929533,
3.59658905474035));
#23393=CARTESIAN_POINT('Ctrl Pts',(3.99203422440346,-0.184112308377066,
3.5547318870523));
#23394=CARTESIAN_POINT('Ctrl Pts',(4.00793950309107,-0.0284797076443847,
3.50528009766423));
#23395=CARTESIAN_POINT('Ctrl Pts',(4.03179742112249,0.212077873916637,3.55216010213054));
#23396=CARTESIAN_POINT('Ctrl Pts',(4.05565533915392,0.400711255741927,3.70851080938071));
#23397=CARTESIAN_POINT('Ctrl Pts',(4.07951325718533,0.49139298320592,3.93615790384083));
#23398=CARTESIAN_POINT('Ctrl Pts',(4.10337117521676,0.461898357851897,4.17940600742409));
#23399=CARTESIAN_POINT('Ctrl Pts',(4.12722909324816,0.319466186301668,4.37878980142624));
#23400=CARTESIAN_POINT('Ctrl Pts',(4.15108701127959,0.0989109688445654,
4.48554634140719));
#23401=CARTESIAN_POINT('Ctrl Pts',(4.174944929311,-0.145828100556353,4.47357507321567));
#23402=CARTESIAN_POINT('Ctrl Pts',(4.19880284734243,-0.354909590370033,
4.34580100620849));
#23403=CARTESIAN_POINT('Ctrl Pts',(4.22266076537384,-0.477205295803391,
4.13346959398438));
#23404=CARTESIAN_POINT('Ctrl Pts',(4.24651868340526,-0.482811689970624,
3.88850100783657));
#23405=CARTESIAN_POINT('Ctrl Pts',(4.27037660143669,-0.370357271909554,
3.67079708031066));
#23406=CARTESIAN_POINT('Ctrl Pts',(4.2942345194681,-0.167340519784032,3.53359217153378));
#23407=CARTESIAN_POINT('Ctrl Pts',(4.31809243749953,0.0765956044913427,
3.51043671457025));
#23408=CARTESIAN_POINT('Ctrl Pts',(4.34195035553093,0.301801986965541,3.60699279882218));
#23409=CARTESIAN_POINT('Ctrl Pts',(4.36580827356237,0.453209578636439,3.79964985833574));
#23410=CARTESIAN_POINT('Ctrl Pts',(4.38966619159377,0.493795074712635,4.04129798000377));
#23411=CARTESIAN_POINT('Ctrl Pts',(4.4135241096252,0.413634228782107,4.27284762322724));
#23412=CARTESIAN_POINT('Ctrl Pts',(4.43738202765661,0.23232854437776,4.43767858897425));
#23413=CARTESIAN_POINT('Ctrl Pts',(4.46123994568804,-0.00578779637616802,
4.49548521832112));
#23414=CARTESIAN_POINT('Ctrl Pts',(4.48509786371945,-0.242488863923451,
4.43213221465579));
#23415=CARTESIAN_POINT('Ctrl Pts',(4.50895578175088,-0.419894798625899,
4.26311111366653));
#23416=CARTESIAN_POINT('Ctrl Pts',(4.53281369978229,-0.494625017545811,
4.02975217827461));
#23417=CARTESIAN_POINT('Ctrl Pts',(4.55667161781372,-0.448405946262215,
3.78911802491887));
#23418=CARTESIAN_POINT('Ctrl Pts',(4.58052953584513,-0.292539406836986,
3.60005025874973));
#23419=CARTESIAN_POINT('Ctrl Pts',(4.60438745387655,-0.0651390137990107,
3.50878109874461));
#23420=CARTESIAN_POINT('Ctrl Pts',(4.62824537190797,0.178189642449287,3.53762834062211));
#23421=CARTESIAN_POINT('Ctrl Pts',(4.65210328993938,0.377946077338085,3.67953804797316));
#23422=CARTESIAN_POINT('Ctrl Pts',(4.67596120797081,0.485284401269169,3.89980943180067));
#23423=CARTESIAN_POINT('Ctrl Pts',(4.69981912600222,0.473957470210434,4.14458013869048));
#23424=CARTESIAN_POINT('Ctrl Pts',(4.72367704403364,0.34673502734182,4.35399706338589));
#23425=CARTESIAN_POINT('Ctrl Pts',(4.74753496206506,0.134726425416229,4.47685206339739));
#23426=CARTESIAN_POINT('Ctrl Pts',(4.77139288009648,-0.110226457398098,
4.48310374471865));
#23427=CARTESIAN_POINT('Ctrl Pts',(4.7952507981279,-0.328225968870003,4.37122340097448));
#23428=CARTESIAN_POINT('Ctrl Pts',(4.81910871615932,-0.465965290257402,
4.16856882376961));
#23429=CARTESIAN_POINT('Ctrl Pts',(4.84296663419074,-0.489763405537152,
3.92469457743051));
#23430=CARTESIAN_POINT('Ctrl Pts',(4.86682455222216,-0.393801027275785,
3.69923455818817));
#23431=CARTESIAN_POINT('Ctrl Pts',(4.89068247025357,-0.201543570920867,
3.54731988215497));
#23432=CARTESIAN_POINT('Ctrl Pts',(4.914540388285,0.039996778460842,3.50609782569371));
#23433=CARTESIAN_POINT('Ctrl Pts',(4.93839830631641,0.271756826018508,3.58564830447545));
#23434=CARTESIAN_POINT('Ctrl Pts',(4.96225622434784,0.437064927107334,3.76651905952651));
#23435=CARTESIAN_POINT('Ctrl Pts',(4.98611414237925,0.495498748108838,4.00448226441646));
#23436=CARTESIAN_POINT('Ctrl Pts',(5.00997206041068,0.432769628082826,4.24134943356216));
#23437=CARTESIAN_POINT('Ctrl Pts',(5.03382997844209,0.26421654558258,4.41920009197534));
#23438=CARTESIAN_POINT('Ctrl Pts',(5.05768789647352,0.031055320573195,4.49454490911931));
#23439=CARTESIAN_POINT('Ctrl Pts',(5.08154581450493,-0.209699776246285,
4.44896002485074));
#23440=CARTESIAN_POINT('Ctrl Pts',(5.10540373253635,-0.399177565666329,
4.29359218508065));
#23441=CARTESIAN_POINT('Ctrl Pts',(5.12926165056777,-0.491045566902382,
4.06643305876778));
#23442=CARTESIAN_POINT('Ctrl Pts',(5.15311956859918,-0.462839551218119,
3.823029239986));
#23443=CARTESIAN_POINT('Ctrl Pts',(5.17697748663061,-0.321456657764784,
3.62289959261435));
#23444=CARTESIAN_POINT('Ctrl Pts',(5.20083540466202,-0.101468855184408,
3.51498126685736));
#23445=CARTESIAN_POINT('Ctrl Pts',(5.22469332269345,0.143330846444675,3.52566323299877));
#23446=CARTESIAN_POINT('Ctrl Pts',(5.24855124072486,0.353082251864168,3.6523334593461));
#23447=CARTESIAN_POINT('Ctrl Pts',(5.27240915875629,0.476495428935435,3.86401762512973));
#23448=CARTESIAN_POINT('Ctrl Pts',(5.2962670767877,0.483392494157105,4.10895318565465));
#23449=CARTESIAN_POINT('Ctrl Pts',(5.32012499481913,0.372086927210194,4.32724672446184));
#23450=CARTESIAN_POINT('Ctrl Pts',(5.34398291285054,0.169795971115995,4.46551952511629));
#23451=CARTESIAN_POINT('Ctrl Pts',(5.36784083088196,-0.0740147250654609,
4.48996012138256));
#23452=CARTESIAN_POINT('Ctrl Pts',(5.39169874891337,-0.299726804847767,
4.39459212172504));
#23453=CARTESIAN_POINT('Ctrl Pts',(5.4155566669448,-0.452147516450583,4.20273559983216));
#23454=CARTESIAN_POINT('Ctrl Pts',(5.43941458497621,-0.494005844030112,
3.96130470137348));
#23455=CARTESIAN_POINT('Ctrl Pts',(5.46327250300764,-0.415066286295368,
3.72933585746768));
#23456=CARTESIAN_POINT('Ctrl Pts',(5.48713042103905,-0.234631715382576,
3.56355176915442));
#23457=CARTESIAN_POINT('Ctrl Pts',(5.51098833907048,0.00317670118048804,
3.50449116189365));
#23458=CARTESIAN_POINT('Ctrl Pts',(5.53484625710188,0.240208327774024,3.56659596294035));
#23459=CARTESIAN_POINT('Ctrl Pts',(5.55870417513332,0.418502475082003,3.73467985673571));
#23460=CARTESIAN_POINT('Ctrl Pts',(5.58256209316472,0.494461367456411,3.96764175273735));
#23461=CARTESIAN_POINT('Ctrl Pts',(5.60642001119615,0.449510986625754,4.20851612161082));
#23462=CARTESIAN_POINT('Ctrl Pts',(5.63027792922757,0.294642925140636,4.39840261889448));
#23463=CARTESIAN_POINT('Ctrl Pts',(5.65413584725899,0.0677266425295592,
4.49086882357174));
#23464=CARTESIAN_POINT('Ctrl Pts',(5.6779937652904,-0.17575064898472,4.46330422991997));
#23465=CARTESIAN_POINT('Ctrl Pts',(5.70185168332183,-0.376252119531055,
4.32244913183746));
#23466=CARTESIAN_POINT('Ctrl Pts',(5.72570960135325,-0.48474969783608,4.10274643779879));
#23467=CARTESIAN_POINT('Ctrl Pts',(5.74956751938466,-0.474712770918799,
3.85791944074229));
#23468=CARTESIAN_POINT('Ctrl Pts',(5.77342543741608,-0.348595640189148,
3.64783501103505));
#23469=CARTESIAN_POINT('Ctrl Pts',(5.7972833554475,-0.13723738064616,3.52386451312966));
#23470=CARTESIAN_POINT('Ctrl Pts',(5.82114127347893,0.1076791581852,3.5163221129105));
#23471=CARTESIAN_POINT('Ctrl Pts',(5.84499919151033,0.326265206982528,3.62705212841851));
#23472=CARTESIAN_POINT('Ctrl Pts',(5.86885710954176,0.465070530553655,3.82897806268729));
#23473=CARTESIAN_POINT('Ctrl Pts',(5.89271502757317,0.490153431381492,4.07272350923538));
#23474=CARTESIAN_POINT('Ctrl Pts',(5.9165729456046,0.395380485146506,4.29868609559117));
#23475=CARTESIAN_POINT('Ctrl Pts',(5.94043086363601,0.203926205561759,4.45161176009809));
#23476=CARTESIAN_POINT('Ctrl Pts',(5.96428878166744,-0.0373935204432717,
4.49410611450448));
#23477=CARTESIAN_POINT('Ctrl Pts',(5.98814669969885,-0.26956963613406,4.41577793841189));
#23478=CARTESIAN_POINT('Ctrl Pts',(6.01200461773027,-0.435828398698505,
4.23578096933615));
#23479=CARTESIAN_POINT('Ctrl Pts',(6.0358625357617,-0.495515688199628,3.99812868033461));
#23480=CARTESIAN_POINT('Ctrl Pts',(6.0597204537931,-0.434035059498629,3.76093483037113));
#23481=CARTESIAN_POINT('Ctrl Pts',(6.08357837182454,-0.266422612259865,
3.58219732064663));
#23482=CARTESIAN_POINT('Ctrl Pts',(6.10743628985594,-0.0336596025775484,
3.50562697870369));
#23483=CARTESIAN_POINT('Ctrl Pts',(6.13129420788738,0.207328476491996,3.54993858195554));
#23484=CARTESIAN_POINT('Ctrl Pts',(6.15515212591877,0.397629707835022,3.70431327123879));
#23485=CARTESIAN_POINT('Ctrl Pts',(6.17901004395022,0.490679606253205,3.93097100878581));
#23486=CARTESIAN_POINT('Ctrl Pts',(6.20286796198161,0.463782811036945,4.17454675550933));
#23487=CARTESIAN_POINT('Ctrl Pts',(6.22672588001306,0.323407044622774,4.3753682944706));
#23488=CARTESIAN_POINT('Ctrl Pts',(6.25058379804445,0.104084330837213,4.48453946106473));
#23489=CARTESIAN_POINT('Ctrl Pts',(6.27444171607588,-0.140944443623038,
4.4749681472433));
#23490=CARTESIAN_POINT('Ctrl Pts',(6.29829963410731,-0.351028389709017,
4.349743491311));
#23491=CARTESIAN_POINT('Ctrl Pts',(6.32215755213872,-0.476177279109797,
4.13807688197341));
#23492=CARTESIAN_POINT('Ctrl Pts',(6.34601547017014,-0.483231738207782,
3.89435343878414));
#23493=CARTESIAN_POINT('Ctrl Pts',(6.37782602754537,-0.338784024988664,
3.5998542259592));
#23494=CARTESIAN_POINT('Ctrl Pts',(6.41758922426439,0.0803770223010952,
3.44371490521648));
#23495=CARTESIAN_POINT('Ctrl Pts',(6.46530506032724,0.512014121509362,3.7673575683149));
#23496=CARTESIAN_POINT('Ctrl Pts',(6.51302089639006,0.472271980317209,4.30452828893312));
#23497=CARTESIAN_POINT('Ctrl Pts',(6.56073673245292,-0.000548856210248058,
4.56210751581942));
#23498=CARTESIAN_POINT('Ctrl Pts',(6.60845256851575,-0.473190198344468,
4.30346185287483));
#23499=CARTESIAN_POINT('Ctrl Pts',(6.65616840457859,-0.511122033036262,
3.76615996983968));
#23500=CARTESIAN_POINT('Ctrl Pts',(6.70388424064142,-0.0797735308749388,
3.44358772816382));
#23501=CARTESIAN_POINT('Ctrl Pts',(6.75160007670426,0.424880365184703,3.63198234005898));
#23502=CARTESIAN_POINT('Ctrl Pts',(6.7993159127671,0.539334593204737,4.15833063512042));
#23503=CARTESIAN_POINT('Ctrl Pts',(6.84703174882994,0.158523065679302,4.53928284691909));
#23504=CARTESIAN_POINT('Ctrl Pts',(6.89474758489278,-0.367869781963911,
4.42500259414721));
#23505=CARTESIAN_POINT('Ctrl Pts',(6.94246342095561,-0.556438361909488,
3.92043630538129));
#23506=CARTESIAN_POINT('Ctrl Pts',(6.99017925701846,-0.234023037562683,
3.48893437735136));
#23507=CARTESIAN_POINT('Ctrl Pts',(7.03789509308128,0.303300305128555,3.52675198254107));
#23508=CARTESIAN_POINT('Ctrl Pts',(7.08561092914413,0.562097748282813,3.99916046672433));
#23509=CARTESIAN_POINT('Ctrl Pts',(7.13332676520696,0.304712478085684,4.47233993757656));
#23510=CARTESIAN_POINT('Ctrl Pts',(7.18104260126981,-0.232495107101315,
4.51176235979777));
#23511=CARTESIAN_POINT('Ctrl Pts',(7.22875843733264,-0.556198774489988,
4.08122554105153));
#23512=CARTESIAN_POINT('Ctrl Pts',(7.27647427339549,-0.369136593294786,
3.57609805363465));
#23513=CARTESIAN_POINT('Ctrl Pts',(7.32419010945832,0.156909424853758,3.46024624852207));
#23514=CARTESIAN_POINT('Ctrl Pts',(7.37190594552116,0.538863091386428,3.84005861730642));
#23515=CARTESIAN_POINT('Ctrl Pts',(7.41962178158399,0.425970496197337,4.36674761950234));
#23516=CARTESIAN_POINT('Ctrl Pts',(7.46733761764684,-0.0780973635293338,
4.55664663921719));
#23517=CARTESIAN_POINT('Ctrl Pts',(7.51505345370967,-0.510447210801067,
4.2353684852172));
#23518=CARTESIAN_POINT('Ctrl Pts',(7.56276928977251,-0.474045531130633,
3.69794782953315));
#23519=CARTESIAN_POINT('Ctrl Pts',(7.61048512583535,-0.00232054557778912,
3.43790632971152));
#23520=CARTESIAN_POINT('Ctrl Pts',(7.65820096189818,0.471535432411473,3.69404409621074));
#23521=CARTESIAN_POINT('Ctrl Pts',(7.70591679796103,0.512373167457076,4.23114587691112));
#23522=CARTESIAN_POINT('Ctrl Pts',(7.75363263402387,0.0826907388754792,
4.55598284219971));
#23523=CARTESIAN_POINT('Ctrl Pts',(7.80134847008669,-0.422927867535356,
4.3702522086048));
#23524=CARTESIAN_POINT('Ctrl Pts',(7.84906430614955,-0.540165305628305,
3.84451327478339));
#23525=CARTESIAN_POINT('Ctrl Pts',(7.89678014221237,-0.161360632039799,
3.46156019320034));
#23526=CARTESIAN_POINT('Ctrl Pts',(7.94449597827521,0.365623992797271,3.57306467116217));
#23527=CARTESIAN_POINT('Ctrl Pts',(7.99221181433806,0.556850479203549,4.07663043084052));
#23528=CARTESIAN_POINT('Ctrl Pts',(8.03992765040089,0.236712602309549,4.50982528676712));
#23529=CARTESIAN_POINT('Ctrl Pts',(8.08764348646373,-0.300802099575971,
4.47483973718518));
#23530=CARTESIAN_POINT('Ctrl Pts',(8.13535932252656,-0.562085604986122,
4.00380155059756));
#23531=CARTESIAN_POINT('Ctrl Pts',(8.18307515858941,-0.307197250538534,
3.52927234160183));
#23532=CARTESIAN_POINT('Ctrl Pts',(8.23079099465223,0.229795065915734,3.48701958438918));
#23533=CARTESIAN_POINT('Ctrl Pts',(8.27850683071509,0.555763037488074,3.91584463605021));
#23534=CARTESIAN_POINT('Ctrl Pts',(8.32622266677791,0.371365260221553,4.42195085332305));
#23535=CARTESIAN_POINT('Ctrl Pts',(8.37393850284076,-0.154062949695418,
4.54057310944092));
#23536=CARTESIAN_POINT('Ctrl Pts',(8.4216543389036,-0.538012782343907,4.16277876137275));
#23537=CARTESIAN_POINT('Ctrl Pts',(8.46937017496643,-0.427897198575242,
3.6355021720628));
#23538=CARTESIAN_POINT('Ctrl Pts',(8.51708601102927,0.0751629666897603,
3.44294954666756));
#23539=CARTESIAN_POINT('Ctrl Pts',(8.56480184709211,0.50919982311266,3.76194492389047));
#23540=CARTESIAN_POINT('Ctrl Pts',(8.61251768315494,0.475630646924824,4.29954994045293));
#23541=CARTESIAN_POINT('Ctrl Pts',(8.66023351921779,0.00528252914771292,
4.56207363752918));
#23542=CARTESIAN_POINT('Ctrl Pts',(8.70794935528062,-0.469916616427902,
4.30843646464781));
#23543=CARTESIAN_POINT('Ctrl Pts',(8.75566519134346,-0.513584102541225,
3.7715573403753));
#23544=CARTESIAN_POINT('Ctrl Pts',(8.8033810274063,-0.0856194047837525,
3.44446062547832));
#23545=CARTESIAN_POINT('Ctrl Pts',(8.85109686346913,0.420970909810523,3.6275242662766));
#23546=CARTESIAN_POINT('Ctrl Pts',(8.89881269953199,0.540977160455745,4.15263810462895));
#23547=CARTESIAN_POINT('Ctrl Pts',(8.9465285355948,0.1641957606509,4.5375820228614));
#23548=CARTESIAN_POINT('Ctrl Pts',(8.99424437165766,-0.363369132636193,
4.42885609773758));
#23549=CARTESIAN_POINT('Ctrl Pts',(9.04196020772048,-0.557246560270691,
3.92630501926208));
#23550=CARTESIAN_POINT('Ctrl Pts',(9.08967604378333,-0.239395897268157,
3.49142917554125));
#23551=CARTESIAN_POINT('Ctrl Pts',(9.13739187984617,0.298295701775085,3.52358174528888));
#23552=CARTESIAN_POINT('Ctrl Pts',(9.18510771590899,0.562057768008922,3.99323652897485));
#23553=CARTESIAN_POINT('Ctrl Pts',(9.23282355197185,0.309673537509763,4.46910231217259));
#23554=CARTESIAN_POINT('Ctrl Pts',(9.28053938803466,-0.227088667424462,
4.51418422403538));
#23555=CARTESIAN_POINT('Ctrl Pts',(9.32825522409753,-0.555311854854516,
4.08708285122523));
#23556=CARTESIAN_POINT('Ctrl Pts',(9.37597106016035,-0.373583621400482,
3.58001195619306));
#23557=CARTESIAN_POINT('Ctrl Pts',(9.4236868962232,0.151212199908504,3.45862254413551));
#23558=CARTESIAN_POINT('Ctrl Pts',(9.47140273228603,0.537147531342748,3.83438837996121));
#23559=CARTESIAN_POINT('Ctrl Pts',(9.51911856834887,0.429812019667804,4.36223791473086));
#23560=CARTESIAN_POINT('Ctrl Pts',(9.5668344044117,-0.0722264831760907,
4.5574387986564));
#23561=CARTESIAN_POINT('Ctrl Pts',(9.61455024047456,-0.507938295172089,
4.24073505647735));
#23562=CARTESIAN_POINT('Ctrl Pts',(9.66226607653738,-0.477202555076283,
3.70296060775017));
#23563=CARTESIAN_POINT('Ctrl Pts',(9.70998191260023,-0.00824436594879979,
3.43796200346455));
#23564=CARTESIAN_POINT('Ctrl Pts',(9.75769774866306,0.46828475128534,3.68909153946361));
#23565=CARTESIAN_POINT('Ctrl Pts',(9.80541358472589,0.514780775927077,4.22573309871483));
#23566=CARTESIAN_POINT('Ctrl Pts',(9.85312942078874,0.0885456931146035,
4.55508048006603));
#23567=CARTESIAN_POINT('Ctrl Pts',(9.90084525685159,-0.419002262135622,
4.37468891556157));
#23568=CARTESIAN_POINT('Ctrl Pts',(9.9485610929144,-0.541773992888202,3.8502147545669));
#23569=CARTESIAN_POINT('Ctrl Pts',(9.99627692897727,-0.167026329707142,
3.46329068919569));
#23570=CARTESIAN_POINT('Ctrl Pts',(10.0439927650401,0.361104182074418,3.56923504227033));
#23571=CARTESIAN_POINT('Ctrl Pts',(10.0917086011029,0.557627167155001,4.07075748419897));
#23572=CARTESIAN_POINT('Ctrl Pts',(10.1394244371657,0.242072544440304,4.50730223964386));
#23573=CARTESIAN_POINT('Ctrl Pts',(10.1871402732286,-0.295781020598791,
4.47798354257549));
#23574=CARTESIAN_POINT('Ctrl Pts',(10.2348561092914,-0.56201432324602,4.00972520363789));
#23575=CARTESIAN_POINT('Ctrl Pts',(10.2825719453543,-0.312141225154507,
3.53253606055812));
#23576=CARTESIAN_POINT('Ctrl Pts',(10.3302877814171,0.224375962906492,3.48462624592509));
#23577=CARTESIAN_POINT('Ctrl Pts',(10.37800361748,0.554845251762499,3.90999207970357));
#23578=CARTESIAN_POINT('Ctrl Pts',(10.4257194535428,0.375791608533427,4.41801357164013));
#23579=CARTESIAN_POINT('Ctrl Pts',(10.4734352896056,-0.148357251109035,
4.54216676877402));
#23580=CARTESIAN_POINT('Ctrl Pts',(10.5211511256685,-0.536267364288337,
4.16843987983467));
#23581=CARTESIAN_POINT('Ctrl Pts',(10.5688669617313,-0.431714905307627,
3.64003205746247));
#23582=CARTESIAN_POINT('Ctrl Pts',(10.6165827977942,0.0692879940047382,
3.44218833554121));
#23583=CARTESIAN_POINT('Ctrl Pts',(10.664298633857,0.50666266228973,3.75659164812817));
#23584=CARTESIAN_POINT('Ctrl Pts',(10.7120144699198,0.478761211786921,4.29452059555793));
#23585=CARTESIAN_POINT('Ctrl Pts',(10.7597303059827,0.0112059738120427,
4.56198674830498));
#23586=CARTESIAN_POINT('Ctrl Pts',(10.8074461420455,-0.466639882340508,
4.31337182280594));
#23587=CARTESIAN_POINT('Ctrl Pts',(10.8551619781083,-0.515963154362253,
3.77698273057893));
#23588=CARTESIAN_POINT('Ctrl Pts',(10.9028778141712,-0.0914695226195351,
3.44539382842306));
#23589=CARTESIAN_POINT('Ctrl Pts',(10.950593650234,0.417021979184216,3.62310830733915));
#23590=CARTESIAN_POINT('Ctrl Pts',(10.9983094862969,0.542555780795161,4.14692822684982));
#23591=CARTESIAN_POINT('Ctrl Pts',(11.0460253223597,0.169852260608159,4.53582169486292));
#23592=CARTESIAN_POINT('Ctrl Pts',(11.0937411584225,-0.358829204008283,
4.43266185580689));
#23593=CARTESIAN_POINT('Ctrl Pts',(11.1414569944853,-0.55799228928692,3.93218197720501));
#23594=CARTESIAN_POINT('Ctrl Pts',(11.1891728305482,-0.244742469498405,
3.49398043245019));
#23595=CARTESIAN_POINT('Ctrl Pts',(11.236888666611,0.293258125877444,3.5204644426882));
#23596=CARTESIAN_POINT('Ctrl Pts',(11.2846045026739,0.561955271903759,3.98731333380864));
#23597=CARTESIAN_POINT('Ctrl Pts',(11.3323203387367,0.314600244947554,4.46581258570203));
#23598=CARTESIAN_POINT('Ctrl Pts',(11.3800361747996,-0.221657027690976,
4.51654897269734));
#23599=CARTESIAN_POINT('Ctrl Pts',(11.4277520108624,-0.554363241169119,
4.0929304899371));
#23600=CARTESIAN_POINT('Ctrl Pts',(11.4754678469252,-0.377989160306769,
3.58397250834823));
#23601=CARTESIAN_POINT('Ctrl Pts',(11.5231836829881,0.145498182576105,3.45705897374896));
#23602=CARTESIAN_POINT('Ctrl Pts',(11.5708995190509,0.535372305622036,3.82873653777755));
#23603=CARTESIAN_POINT('Ctrl Pts',(11.6186153551137,0.43360580265347,4.35768797439208));
#23604=CARTESIAN_POINT('Ctrl Pts',(11.6663311911766,-0.0663475807746441,
4.55816904038548));
#23605=CARTESIAN_POINT('Ctrl Pts',(11.7140470272394,-0.505372959888646,
4.24607488805821));
#23606=CARTESIAN_POINT('Ctrl Pts',(11.7617628633023,-0.480306573774387,
3.70800637967828));
#23607=CARTESIAN_POINT('Ctrl Pts',(11.8094786993651,-0.0141672704965164,
3.43808010573911));
#23608=CARTESIAN_POINT('Ctrl Pts',(11.8571945354279,0.464982055269784,3.68417351694868));
#23609=CARTESIAN_POINT('Ctrl Pts',(11.9049103714908,0.517131205013274,4.22029524715934));
#23610=CARTESIAN_POINT('Ctrl Pts',(11.9526262075536,0.0943908121067024,
4.55411646222552));
#23611=CARTESIAN_POINT('Ctrl Pts',(12.0003420436165,-0.415030115946784,
4.37908400385228));
#23612=CARTESIAN_POINT('Ctrl Pts',(12.0480578796793,-0.543322502467158,
3.85593287178435));
#23613=CARTESIAN_POINT('Ctrl Pts',(12.0957737157421,-0.172673474880652,
3.46508080031456));
#23614=CARTESIAN_POINT('Ctrl Pts',(12.143489551805,0.356544261611682,3.56545326070575));
#23615=CARTESIAN_POINT('Ctrl Pts',(12.1912053878678,0.558341916527368,4.06487667815191));
#23616=CARTESIAN_POINT('Ctrl Pts',(12.2389212239306,0.247405598301292,4.50472284379514));
#23617=CARTESIAN_POINT('Ctrl Pts',(12.2866370599935,-0.290727087669313,
4.48107425582212));
#23618=CARTESIAN_POINT('Ctrl Pts',(12.3343528960563,-0.56188061562194,4.01564777644873));
#23619=CARTESIAN_POINT('Ctrl Pts',(12.3820687321191,-0.317050528604376,
3.5358517031905));
#23620=CARTESIAN_POINT('Ctrl Pts',(12.429784568182,0.218931937280033,3.48229015273196));
#23621=CARTESIAN_POINT('Ctrl Pts',(12.4775004042448,0.553865836459325,3.90414952100961));
#23622=CARTESIAN_POINT('Ctrl Pts',(12.5252162403077,0.380176215696692,4.4140298589933));
#23623=CARTESIAN_POINT('Ctrl Pts',(12.5729320763705,-0.142635073703209,
4.54370020679522));
#23624=CARTESIAN_POINT('Ctrl Pts',(12.6206479124333,-0.53446238019874,4.17408228879405));
#23625=CARTESIAN_POINT('Ctrl Pts',(12.6683637484962,-0.435484659196984,
3.644601926393));
#23626=CARTESIAN_POINT('Ctrl Pts',(12.716079584559,0.0634053251381518,3.44148908348752));
#23627=CARTESIAN_POINT('Ctrl Pts',(12.7637954206219,0.504069223782589,3.75126540901054));
#23628=CARTESIAN_POINT('Ctrl Pts',(12.8115112566847,0.481838598125516,4.2894585367128));
#23629=CARTESIAN_POINT('Ctrl Pts',(12.8592270927475,0.0171281737699642,
4.56183743625962));
#23630=CARTESIAN_POINT('Ctrl Pts',(12.9069429288104,-0.463311316109371,
4.31827237310907));
#23631=CARTESIAN_POINT('Ctrl Pts',(12.9546587648732,-0.518284895444539,
3.78243289248252));
#23632=CARTESIAN_POINT('Ctrl Pts',(13.0023746009361,-0.0973094804548018,
3.44638863438952));
#23633=CARTESIAN_POINT('Ctrl Pts',(13.0500904369989,0.413026727735397,3.61873421174243));
#23634=CARTESIAN_POINT('Ctrl Pts',(13.0978062730617,0.544074136613086,4.14120202898048));
#23635=CARTESIAN_POINT('Ctrl Pts',(13.1455221091246,0.17548989418231,4.53400185033327));
#23636=CARTESIAN_POINT('Ctrl Pts',(13.1932379451874,-0.354249418335187,
4.4364195558504));
#23637=CARTESIAN_POINT('Ctrl Pts',(13.2409537812502,-0.558676039167545,
3.93806646805208));
#23638=CARTESIAN_POINT('Ctrl Pts',(13.2886696173131,-0.250061856896528,
3.49658789561142));
#23639=CARTESIAN_POINT('Ctrl Pts',(13.3363854533759,0.288187976258808,3.51740040462167));
#23640=CARTESIAN_POINT('Ctrl Pts',(13.3841012894388,0.56179035647369,3.9813915478171));
#23641=CARTESIAN_POINT('Ctrl Pts',(13.4318171255016,0.319492008083037,4.46247111897993));
#23642=CARTESIAN_POINT('Ctrl Pts',(13.4795329615644,-0.21620076734671,4.51885634555065));
#23643=CARTESIAN_POINT('Ctrl Pts',(13.5272487976273,-0.553353051445561,
4.09876780637113));
#23644=CARTESIAN_POINT('Ctrl Pts',(13.5749646336901,-0.382352713970831,
3.58797927086295));
#23645=CARTESIAN_POINT('Ctrl Pts',(13.6226804697529,0.139768003996038,3.45555571067516));
#23646=CARTESIAN_POINT('Ctrl Pts',(13.6703963058158,0.53353761328617,3.82310371872654));
#23647=CARTESIAN_POINT('Ctrl Pts',(13.7181121418786,0.437351422764197,4.35309830377052));
#23648=CARTESIAN_POINT('Ctrl Pts',(13.7658279779415,-0.0604613087987784,
4.55883728334624));
#23649=CARTESIAN_POINT('Ctrl Pts',(13.8135438140043,-0.502751490175015,
4.25138738680826));
#23650=CARTESIAN_POINT('Ctrl Pts',(13.8612596500671,-0.483357242297515,
3.71308458487209));
#23651=CARTESIAN_POINT('Ctrl Pts',(13.90897548613,-0.0200886014110514,3.43826062340902));
#23652=CARTESIAN_POINT('Ctrl Pts',(13.9566913221928,0.461627711254046,3.67929057494076));
#23653=CARTESIAN_POINT('Ctrl Pts',(14.0044071582557,0.519424193619207,4.21483292625321));
#23654=CARTESIAN_POINT('Ctrl Pts',(14.0521229943185,0.100225446615308,4.55309089575788));
#23655=CARTESIAN_POINT('Ctrl Pts',(14.0998388303813,-0.411011870182152,
4.38343698529073));
#23656=CARTESIAN_POINT('Ctrl Pts',(14.1475546664441,-0.544810662360815,
3.86166699129474));
#23657=CARTESIAN_POINT('Ctrl Pts',(14.195270502507,-0.178301440303968,3.46693032771971));
#23658=CARTESIAN_POINT('Ctrl Pts',(14.2429863385698,0.351944737904315,3.5617197465309));
#23659=CARTESIAN_POINT('Ctrl Pts',(14.2907021746327,0.558994647929194,4.05898866591129));
#23660=CARTESIAN_POINT('Ctrl Pts',(14.3384180106955,0.252711171522458,4.50208738572805));
#23661=CARTESIAN_POINT('Ctrl Pts',(14.3861338467583,-0.28564086215454,4.48411153362329));
#23662=CARTESIAN_POINT('Ctrl Pts',(14.4338496828212,-0.561684496965419,
4.02156861117883));
#23663=CARTESIAN_POINT('Ctrl Pts',(14.481565518884,-0.321924615586062,3.53921890121312));
#23664=CARTESIAN_POINT('Ctrl Pts',(14.5292813549469,0.213463593732893,3.48001156429194));
#23665=CARTESIAN_POINT('Ctrl Pts',(14.5769971910097,0.552824900367352,3.89831760893199));
#23666=CARTESIAN_POINT('Ctrl Pts',(14.6247130270725,0.384518594689996,4.4100001578745));
#23667=CARTESIAN_POINT('Ctrl Pts',(14.6724288631354,-0.136897053070264,
4.54517325317752));
#23668=CARTESIAN_POINT('Ctrl Pts',(14.7201446991982,-0.532598030564186,
4.17970536151887));
#23669=CARTESIAN_POINT('Ctrl Pts',(14.7678605352611,-0.439206041516937,
3.64921127125505));
#23670=CARTESIAN_POINT('Ctrl Pts',(14.8155763713239,0.0575156135089261,
3.44085186817608));
#23671=CARTESIAN_POINT('Ctrl Pts',(14.8632922073868,0.501419795658073,3.74596679815093));
#23672=CARTESIAN_POINT('Ctrl Pts',(14.9110080434496,0.484862464119148,4.284364326187));
#23673=CARTESIAN_POINT('Ctrl Pts',(14.9587238795124,0.0230484712116303,
4.56162571797798));
#23674=CARTESIAN_POINT('Ctrl Pts',(15.0064397155752,-0.459931287455839,
4.32313757122732));
#23675=CARTESIAN_POINT('Ctrl Pts',(15.0541555516381,-0.5205490679001,3.78790722070797));
#23676=CARTESIAN_POINT('Ctrl Pts',(15.1018713877009,-0.103138629614742,
3.44744493287938));
#23677=CARTESIAN_POINT('Ctrl Pts',(15.1495872237638,0.40898559923764,3.61440246534021));
#23678=CARTESIAN_POINT('Ctrl Pts',(15.1973030598266,0.545532059257757,4.13546014705983));
#23679=CARTESIAN_POINT('Ctrl Pts',(15.2450188958894,0.181108035171788,4.53212269141213));
#23680=CARTESIAN_POINT('Ctrl Pts',(15.2927347319523,-0.349630284317748,
4.44012878048063));
#23681=CARTESIAN_POINT('Ctrl Pts',(15.3404505680151,-0.559297733964875,
3.94395783818199));
#23682=CARTESIAN_POINT('Ctrl Pts',(15.3881664040779,-0.255353468610234,
3.49925127540033));
#23683=CARTESIAN_POINT('Ctrl Pts',(15.4358822401408,0.283085816087337,3.51438997142805));
#23684=CARTESIAN_POINT('Ctrl Pts',(15.4835980762036,0.561563040036739,3.97547182876414));
#23685=CARTESIAN_POINT('Ctrl Pts',(15.5313139122665,0.324348283562367,4.45907828316053));
#23686=CARTESIAN_POINT('Ctrl Pts',(15.5790297483293,-0.210720492447169,
4.52110608630326));
#23687=CARTESIAN_POINT('Ctrl Pts',(15.6267455843921,-0.552281397890927,
4.10459415214592));
#23688=CARTESIAN_POINT('Ctrl Pts',(15.674461420455,-0.386673797709831,3.59203179868507));
#23689=CARTESIAN_POINT('Ctrl Pts',(15.7221772565178,0.134022300649356,3.45411292188939));
#23690=CARTESIAN_POINT('Ctrl Pts',(15.7698930925807,0.531643658124066,3.81749054847505));
#23691=CARTESIAN_POINT('Ctrl Pts',(15.8176089286435,0.441048463954279,4.34846941266494));
#23692=CARTESIAN_POINT('Ctrl Pts',(15.8653247647064,-0.054568321067637,
4.5594434533135));
#23693=CARTESIAN_POINT('Ctrl Pts',(15.9130406007692,-0.500074177211609,
4.25667196264028));
#23694=CARTESIAN_POINT('Ctrl Pts',(15.960756436832,-0.486354221791887,3.71819465926869));
#23695=CARTESIAN_POINT('Ctrl Pts',(16.0084722728949,-0.0260077009790528,
3.4385035364232));
#23696=CARTESIAN_POINT('Ctrl Pts',(16.0561881089577,0.458222091822753,3.6744432558139));
#23697=CARTESIAN_POINT('Ctrl Pts',(16.1039039450206,0.52165948705058,4.2093467427251));
#23698=CARTESIAN_POINT('Ctrl Pts',(16.1516197810833,0.106048948556897,4.55200389457816));
#23699=CARTESIAN_POINT('Ctrl Pts',(16.1993356171462,-0.406947971169398,
4.38774737636841));
#23700=CARTESIAN_POINT('Ctrl Pts',(16.247051453209,-0.546238307271431,3.86741647617928));
#23701=CARTESIAN_POINT('Ctrl Pts',(16.2947672892719,-0.183909600849411,
3.46883906597446));
#23702=CARTESIAN_POINT('Ctrl Pts',(16.3424831253347,0.347306121845567,3.55803491444678));
#23703=CARTESIAN_POINT('Ctrl Pts',(16.3901989613975,0.559585288858183,4.05309410148958));
#23704=CARTESIAN_POINT('Ctrl Pts',(16.4379147974604,0.257988674785898,4.49939615817675));
#23705=CARTESIAN_POINT('Ctrl Pts',(16.4856306335232,-0.280522909008289,
4.4870950386126));
#23706=CARTESIAN_POINT('Ctrl Pts',(16.5333464695861,-0.561425989060384,
4.02748705016995));
#23707=CARTESIAN_POINT('Ctrl Pts',(16.5810623056489,-0.326762944709103,
3.54263728061361));
#23708=CARTESIAN_POINT('Ctrl Pts',(16.6287781417117,0.207971539662738,3.4777907336998));
#23709=CARTESIAN_POINT('Ctrl Pts',(16.6764939777746,0.551722559108811,3.89249699125187));
#23710=CARTESIAN_POINT('Ctrl Pts',(16.7242098138374,0.388818263182495,4.40592491588375));
#23711=CARTESIAN_POINT('Ctrl Pts',(16.7719256499003,-0.131143826562283,
4.54658574430191));
#23712=CARTESIAN_POINT('Ctrl Pts',(16.8196414859631,-0.53067452246778,4.18530847342493));
#23713=CARTESIAN_POINT('Ctrl Pts',(16.8673573220259,-0.442878638914007,
3.65385958006445));
#23714=CARTESIAN_POINT('Ctrl Pts',(16.9150731580888,0.0516195133182915,
3.44027676038576));
#23715=CARTESIAN_POINT('Ctrl Pts',(16.9627889941516,0.498714672202087,3.74069640409388));
#23716=CARTESIAN_POINT('Ctrl Pts',(17.0105048302145,0.487832473891125,4.27923852982128));
#23717=CARTESIAN_POINT('Ctrl Pts',(17.0582206662773,0.0289662085384809,
4.56135161697672));
#23718=CARTESIAN_POINT('Ctrl Pts',(17.1059365023401,-0.456500171817451,
4.32796687675757));
#23719=CARTESIAN_POINT('Ctrl Pts',(17.1536523384029,-0.522755420235406,
3.79340510719289));
#23720=CARTESIAN_POINT('Ctrl Pts',(17.2013681744658,-0.108956322625149,
3.44856260656401));
#23721=CARTESIAN_POINT('Ctrl Pts',(17.2490840105286,0.404899042560309,3.61011354928233));
#23722=CARTESIAN_POINT('Ctrl Pts',(17.2967998465915,0.54692938679005,4.12970321886885));
#23723=CARTESIAN_POINT('Ctrl Pts',(17.3445156826543,0.186706059540143,4.53018442682757));
#23724=CARTESIAN_POINT('Ctrl Pts',(17.3922315187172,-0.344972315027459,
4.4437891176945));
#23725=CARTESIAN_POINT('Ctrl Pts',(17.43994735478,-0.559857304624004,3.94985543320929));
#23726=CARTESIAN_POINT('Ctrl Pts',(17.4876631908428,-0.260616716872392,
3.5019702759813));
#23727=CARTESIAN_POINT('Ctrl Pts',(17.5353790269057,0.277952212086773,3.51143347749201));
#23728=CARTESIAN_POINT('Ctrl Pts',(17.5830948629685,0.561273347842132,3.96955483418404));
#23729=CARTESIAN_POINT('Ctrl Pts',(17.6308106990313,0.329168531973526,4.45563445510394));
#23730=CARTESIAN_POINT('Ctrl Pts',(17.6785265350942,-0.205216811715269,
4.52329794506467));
#23731=CARTESIAN_POINT('Ctrl Pts',(17.726242371157,-0.551148399539408,4.11040888009862));
#23732=CARTESIAN_POINT('Ctrl Pts',(17.7739582072198,-0.390951931558304,
3.59612964167903));
#23733=CARTESIAN_POINT('Ctrl Pts',(17.8216740432827,0.128261710741471,3.45273076764982));
#23734=CARTESIAN_POINT('Ctrl Pts',(17.8693898793456,0.529690650507269,3.81189765050732));
#23735=CARTESIAN_POINT('Ctrl Pts',(17.9171057154083,0.44469651557395,4.34380181523062));
#23736=CARTESIAN_POINT('Ctrl Pts',(17.9648215514712,-0.0486692721463468,
4.55998748295674));
#23737=CARTESIAN_POINT('Ctrl Pts',(18.012537387534,-0.497341318381634,4.26192802856871));
#23738=CARTESIAN_POINT('Ctrl Pts',(18.0602532235969,-0.489297179367249,
3.72333603526529));
#23739=CARTESIAN_POINT('Ctrl Pts',(18.1079690596597,-0.0319239117350811,
3.43880881780002));
#23740=CARTESIAN_POINT('Ctrl Pts',(18.1556848957225,0.454765575255941,3.66963209798526));
#23741=CARTESIAN_POINT('Ctrl Pts',(18.2034007317854,0.523836837021606,4.20383730595423));
#23742=CARTESIAN_POINT('Ctrl Pts',(18.2511165678483,0.111860671084556,4.5508555794253));
#23743=CARTESIAN_POINT('Ctrl Pts',(18.298832403911,-0.402838870307115,4.39201469830757));
#23744=CARTESIAN_POINT('Ctrl Pts',(18.346548239974,-0.547605278623001,3.87318068781251));
#23745=CARTESIAN_POINT('Ctrl Pts',(18.3942640760367,-0.189497333589109,
3.47080680306518));
#23746=CARTESIAN_POINT('Ctrl Pts',(18.4419799120997,0.342628928670919,3.55439917374707));
#23747=CARTESIAN_POINT('Ctrl Pts',(18.4896957481624,0.560113773708727,4.04719363962704));
#23748=CARTESIAN_POINT('Ctrl Pts',(18.5374115842253,0.263237521891608,4.49664946007004));
#23749=CARTESIAN_POINT('Ctrl Pts',(18.5851274202881,-0.275373796708506,
4.49002443939646));
#23750=CARTESIAN_POINT('Ctrl Pts',(18.632843256351,-0.561105120620647,4.03340243603));
#23751=CARTESIAN_POINT('Ctrl Pts',(18.6805590924138,-0.331564978554912,
3.54610646169455));
#23752=CARTESIAN_POINT('Ctrl Pts',(18.7282749284766,0.202456385100939,3.47562790763498));
#23753=CARTESIAN_POINT('Ctrl Pts',(18.7759907645394,0.550558935126376,3.8866883144956));
#23754=CARTESIAN_POINT('Ctrl Pts',(18.8237066006023,0.393074743587739,4.40180458567998));
#23755=CARTESIAN_POINT('Ctrl Pts',(18.8714224366651,-0.125376033221007,
4.54793752327491));
#23756=CARTESIAN_POINT('Ctrl Pts',(18.919138272728,-0.528692069562509,4.19089100214638));
#23757=CARTESIAN_POINT('Ctrl Pts',(18.9668541087908,-0.4465020434557,3.6585463365067));
#23758=CARTESIAN_POINT('Ctrl Pts',(19.0145699448537,0.0457176794812401,
3.43976382400136));
#23759=CARTESIAN_POINT('Ctrl Pts',(19.0622857809165,0.495954153879041,3.73545481224116));
#23760=CARTESIAN_POINT('Ctrl Pts',(19.1100016169793,0.490748297561716,4.27408171698104));
#23761=CARTESIAN_POINT('Ctrl Pts',(19.1577174530421,0.0348807284082936,
4.5610151636709));
#23762=CARTESIAN_POINT('Ctrl Pts',(19.205433289105,-0.453018350253257,4.33275975334162));
#23763=CARTESIAN_POINT('Ctrl Pts',(19.2531491251678,-0.524903707479367,
3.79892594114836));
#23764=CARTESIAN_POINT('Ctrl Pts',(19.3008649612307,-0.11476191309534,3.44974153150476));
#23765=CARTESIAN_POINT('Ctrl Pts',(19.3485807972935,0.400767511262006,3.60586793956989));
#23766=CARTESIAN_POINT('Ctrl Pts',(19.3962966333564,0.548265964675035,4.12393188459875));
#23767=CARTESIAN_POINT('Ctrl Pts',(19.4440124694192,0.192283344213529,4.52818727047755));
#23768=CARTESIAN_POINT('Ctrl Pts',(19.491728305482,-0.340276025447905,4.44740016355363));
#23769=CARTESIAN_POINT('Ctrl Pts',(19.5394441415448,-0.560354693525076,
3.95575859308266));
#23770=CARTESIAN_POINT('Ctrl Pts',(19.5871599776077,-0.265851008504119,
3.50474460473346));
#23771=CARTESIAN_POINT('Ctrl Pts',(19.6348758136705,0.272787718306182,3.5085312334714));
#23772=CARTESIAN_POINT('Ctrl Pts',(19.6825916497334,0.560921342594646,3.96364125479661));
#23773=CARTESIAN_POINT('Ctrl Pts',(19.7303074857962,0.33395216026474,4.45213995410186));
#23774=CARTESIAN_POINT('Ctrl Pts',(19.7780233218591,-0.199690227635008,
4.52543179776919));
#23775=CARTESIAN_POINT('Ctrl Pts',(19.8257391579219,-0.549954387748789,
4.11621111891367));
#23776=CARTESIAN_POINT('Ctrl Pts',(19.8734549939848,-0.395186252277308,
3.60027277035845));
#23777=CARTESIAN_POINT('Ctrl Pts',(19.9211708300475,0.122486141425193,3.45140859770427));
#23778=CARTESIAN_POINT('Ctrl Pts',(19.9688866661104,0.527680190865048,3.80632716374734));
#23779=CARTESIAN_POINT('Ctrl Pts',(20.0166025021732,0.448292560087992,4.33909316421112));
#23780=CARTESIAN_POINT('Ctrl Pts',(20.0643183382361,-0.0427598846646947,
4.56047472290141));
#23781=CARTESIAN_POINT('Ctrl Pts',(20.1120341742989,-0.49456253103916,4.26714478353561));
#23782=CARTESIAN_POINT('Ctrl Pts',(20.1597500103618,-0.492168201513856,
3.72852743457374));
#23783=CARTESIAN_POINT('Ctrl Pts',(20.2074658464246,-0.0378697858522375,
3.43914000028616));
#23784=CARTESIAN_POINT('Ctrl Pts',(20.2551816824874,0.451321269441671,3.66492646727415));
#23785=CARTESIAN_POINT('Ctrl Pts',(20.3028975185503,0.52583741886325,4.1981749506787));
#23786=CARTESIAN_POINT('Ctrl Pts',(20.3506133546131,0.117885080656874,4.54989459844945));
#23787=CARTESIAN_POINT('Ctrl Pts',(20.398329190676,-0.399119892637424,4.39574851066478));
#23788=CARTESIAN_POINT('Ctrl Pts',(20.438092387395,-0.523197416260526,3.96600412247733));
#23789=CARTESIAN_POINT('Ctrl Pts',(20.4699029447702,-0.3725623900923,3.67462118354637));
#23790=CARTESIAN_POINT('Ctrl Pts',(20.4937608628016,-0.172533290246804,
3.53519650363565));
#23791=CARTESIAN_POINT('Ctrl Pts',(20.5176187808331,0.0720421502968434,
3.50974356844941));
#23792=CARTESIAN_POINT('Ctrl Pts',(20.5414766988645,0.297725647320748,3.60399556061657));
#23793=CARTESIAN_POINT('Ctrl Pts',(20.5653346168959,0.451286063531533,3.79517586539437));
#23794=CARTESIAN_POINT('Ctrl Pts',(20.5891925349273,0.494134760388362,4.03639109206021));
#23795=CARTESIAN_POINT('Ctrl Pts',(20.6130504529587,0.416344747430809,4.26873428690612));
#23796=CARTESIAN_POINT('Ctrl Pts',(20.6369083709901,0.23664610161733,4.43535054865035));
#23797=CARTESIAN_POINT('Ctrl Pts',(20.6607662890216,-0.000865470816140784,
4.49551919950567));
#23798=CARTESIAN_POINT('Ctrl Pts',(20.684624207053,-0.238193741375527,4.43451595913869));
#23799=CARTESIAN_POINT('Ctrl Pts',(20.7084821250844,-0.417262150572256,
4.26726382233879));
#23800=CARTESIAN_POINT('Ctrl Pts',(20.7323400431158,-0.494306543785295,
4.03465729316116));
#23801=CARTESIAN_POINT('Ctrl Pts',(20.7561979611472,-0.45047531426282,3.79357669839993));
#23802=CARTESIAN_POINT('Ctrl Pts',(20.7800558791787,-0.296492828349621,
3.60297191305088));
#23803=CARTESIAN_POINT('Ctrl Pts',(20.80391379721,-0.0700085893017688,3.50945147432983));
#23804=CARTESIAN_POINT('Ctrl Pts',(20.8277717152415,0.173594031734132,3.53588342526713));
#23805=CARTESIAN_POINT('Ctrl Pts',(20.8516296332729,0.374748514455718,3.6758045671588));
#23806=CARTESIAN_POINT('Ctrl Pts',(20.8754875513043,0.484266602122282,3.89500029884494));
#23807=CARTESIAN_POINT('Ctrl Pts',(20.8993454693358,0.475368407265908,4.13987133054223));
#23808=CARTESIAN_POINT('Ctrl Pts',(20.9232033873671,0.350229638882089,4.35054000504804));
#23809=CARTESIAN_POINT('Ctrl Pts',(20.9470613053986,0.139450209771325,4.47549210343221));
#23810=CARTESIAN_POINT('Ctrl Pts',(20.97091922343,-0.105428607968738,4.48417342845956));
#23811=CARTESIAN_POINT('Ctrl Pts',(20.9947771414615,-0.324527251938122,
4.37446116262749));
#23812=CARTESIAN_POINT('Ctrl Pts',(21.0186350594928,-0.464270146732381,
4.17318294187641));
#23813=CARTESIAN_POINT('Ctrl Pts',(21.0424929775243,-0.490486342136868,
3.92955677471355));
#23814=CARTESIAN_POINT('Ctrl Pts',(21.0663508955557,-0.396765267394252,
3.7031558948169));
#23815=CARTESIAN_POINT('Ctrl Pts',(21.0902088135871,-0.206024276530194,
3.54934148458869));
#23816=CARTESIAN_POINT('Ctrl Pts',(21.1140667316185,0.0350952616297792,
3.50572535702762));
#23817=CARTESIAN_POINT('Ctrl Pts',(21.1379246496499,0.267633052506714,3.58297284346672));
#23818=CARTESIAN_POINT('Ctrl Pts',(21.1617825676814,0.434727271782411,3.76219482925797));
#23819=CARTESIAN_POINT('Ctrl Pts',(21.1856404857128,0.495518831419392,3.99956665698474));
#23820=CARTESIAN_POINT('Ctrl Pts',(21.2094984037442,0.43514253908843,4.23704444887943));
#23821=CARTESIAN_POINT('Ctrl Pts',(21.2333563217756,0.268362042918248,4.41655841606373));
#23822=CARTESIAN_POINT('Ctrl Pts',(21.257214239807,0.0359597172125542,4.49421250369607));
#23823=CARTESIAN_POINT('Ctrl Pts',(21.2810721578384,-0.205235738871087,
4.45101817209691));
#23824=CARTESIAN_POINT('Ctrl Pts',(21.3049300758699,-0.396245466293343,
4.29753761193144));
#23825=CARTESIAN_POINT('Ctrl Pts',(21.3287879939013,-0.490362383696085,
4.07130100088706));
#23826=CARTESIAN_POINT('Ctrl Pts',(21.3526459119327,-0.464572341082516,
3.82762935292545));
#23827=CARTESIAN_POINT('Ctrl Pts',(21.3765038299641,-0.325181706377507,
3.62610702345576));
#23828=CARTESIAN_POINT('Ctrl Pts',(21.4003617479955,-0.106275286691508,
3.51601171139131));
#23829=CARTESIAN_POINT('Ctrl Pts',(21.424219666027,0.138618335471326,3.52426471946798));
#23830=CARTESIAN_POINT('Ctrl Pts',(21.4480775840584,0.349615998723735,3.64884796240357));
#23831=CARTESIAN_POINT('Ctrl Pts',(21.4719355020898,0.475123026939619,3.85929744372095));
#23832=CARTESIAN_POINT('Ctrl Pts',(21.4957934201212,0.484449532977353,4.10415253270923));
#23833=CARTESIAN_POINT('Ctrl Pts',(21.5196513381527,0.375314932061802,4.32353949039209));
#23834=CARTESIAN_POINT('Ctrl Pts',(21.543509256184,0.174405606883644,4.4638122296353));
#23835=CARTESIAN_POINT('Ctrl Pts',(21.5673671742155,-0.069150639890911,
4.49067024474121));
#23836=CARTESIAN_POINT('Ctrl Pts',(21.5912250922469,-0.29579767158652,4.39754601941878));
#23837=CARTESIAN_POINT('Ctrl Pts',(21.6150830102783,-0.450114115212426,
4.20721096341231));
#23838=CARTESIAN_POINT('Ctrl Pts',(21.6389409283097,-0.494365396806572,
3.96620718253823));
#23839=CARTESIAN_POINT('Ctrl Pts',(21.6627988463412,-0.417730872638478,
3.73346666603139));
#23840=CARTESIAN_POINT('Ctrl Pts',(21.6866567643726,-0.238949771349764,
3.56590080990214));
#23841=CARTESIAN_POINT('Ctrl Pts',(21.710514682404,-0.00173894210493873,
3.50448403037633));
#23842=CARTESIAN_POINT('Ctrl Pts',(21.7343726004354,0.235897105852373,3.56423440300754));
#23843=CARTESIAN_POINT('Ctrl Pts',(21.7582305184669,0.415849885720624,3.73054133411992));
#23844=CARTESIAN_POINT('Ctrl Pts',(21.7820884364982,0.49411604100673,3.96273824894669));
#23845=CARTESIAN_POINT('Ctrl Pts',(21.8059463545297,0.451557364815975,4.20404667689569));
#23846=CARTESIAN_POINT('Ctrl Pts',(21.8298042725611,0.29858061275206,4.39546013422383));
#23847=CARTESIAN_POINT('Ctrl Pts',(21.8536621905925,0.0725927676976751,
4.49017281661646));
#23848=CARTESIAN_POINT('Ctrl Pts',(21.8775201086239,-0.171145986446082,
4.46502489330693));
#23849=CARTESIAN_POINT('Ctrl Pts',(21.9013780266554,-0.373034884980705,
4.32616571656009));
#23850=CARTESIAN_POINT('Ctrl Pts',(21.9252359446868,-0.483706592871294,
4.10755013753858));
#23851=CARTESIAN_POINT('Ctrl Pts',(21.9490938627182,-0.476098862901817,
3.86263562028194));
#23852=CARTESIAN_POINT('Ctrl Pts',(21.9729517807496,-0.352071992280181,
3.65131043559696));
#23853=CARTESIAN_POINT('Ctrl Pts',(21.996809698781,-0.141953929297546,3.52524934752154));
#23854=CARTESIAN_POINT('Ctrl Pts',(22.0206676168125,0.102875736145779,3.51527772592526));
#23855=CARTESIAN_POINT('Ctrl Pts',(22.0445255348438,0.322549481822576,3.62383390390986));
#23856=CARTESIAN_POINT('Ctrl Pts',(22.0683834528753,0.46335109312246,3.82437293894729));
#23857=CARTESIAN_POINT('Ctrl Pts',(22.0922413709067,0.490850740723195,4.06785757439707));
#23858=CARTESIAN_POINT('Ctrl Pts',(22.1160992889381,0.398324011712033,4.29474918450382));
#23859=CARTESIAN_POINT('Ctrl Pts',(22.1399572069695,0.208396211707814,4.44956659019228));
#23860=CARTESIAN_POINT('Ctrl Pts',(22.163815125001,-0.0324901386554863,
4.49445271863166));
#23861=CARTESIAN_POINT('Ctrl Pts',(22.1876730430324,-0.265431765108271,
4.41843168874211));
#23862=CARTESIAN_POINT('Ctrl Pts',(22.2115309610638,-0.433468094767725,
4.24009271310828));
#23863=CARTESIAN_POINT('Ctrl Pts',(22.2353888790952,-0.495509667838209,
4.00304452911861));
#23864=CARTESIAN_POINT('Ctrl Pts',(22.2592467971266,-0.436385629680506,
3.76525187484075));
#23865=CARTESIAN_POINT('Ctrl Pts',(22.2831047151581,-0.270553418215538,
3.58486153155103));
#23866=CARTESIAN_POINT('Ctrl Pts',(22.3069626331895,-0.0385635261649252,
3.50598385198694));
#23867=CARTESIAN_POINT('Ctrl Pts',(22.3308205512209,0.202856198284482,3.54790657725669));
#23868=CARTESIAN_POINT('Ctrl Pts',(22.3546784692523,0.394672056935096,3.70037845932536));
#23869=CARTESIAN_POINT('Ctrl Pts',(22.3785363872837,0.489979846308564,3.9261159693126));
#23870=CARTESIAN_POINT('Ctrl Pts',(22.4023943053151,0.465474217808745,4.1699201379362));
#23871=CARTESIAN_POINT('Ctrl Pts',(22.4262522233466,0.327147461276091,4.37217420322137));
#23872=CARTESIAN_POINT('Ctrl Pts',(22.450110141378,0.108824243893236,4.4834215400391));
#23873=CARTESIAN_POINT('Ctrl Pts',(22.4739680594094,-0.136109474402841,
4.47645913832327));
#23874=CARTESIAN_POINT('Ctrl Pts',(22.4978259774408,-0.347760701725541,
4.3529895060813));
#23875=CARTESIAN_POINT('Ctrl Pts',(22.5216838954723,-0.474374996640319,
4.1432043106148));
#23876=CARTESIAN_POINT('Ctrl Pts',(22.5455418135036,-0.484991622785221,
3.89840178635216));
#23877=CARTESIAN_POINT('Ctrl Pts',(22.5693997315351,-0.377014700254462,
3.67844274379546));
#23878=CARTESIAN_POINT('Ctrl Pts',(22.5932576495665,-0.176847198578467,
3.53711330196678));
#23879=CARTESIAN_POINT('Ctrl Pts',(22.6171155675979,0.0665638539184235,
3.50897209184919));
#23880=CARTESIAN_POINT('Ctrl Pts',(22.6409734856293,0.293698998435555,3.60090091054846));
#23881=CARTESIAN_POINT('Ctrl Pts',(22.6648314036608,0.449015288492166,3.79041970485759));
#23882=CARTESIAN_POINT('Ctrl Pts',(22.6886893216922,0.494537845944295,4.03118776656693));
#23883=CARTESIAN_POINT('Ctrl Pts',(22.7125472397236,0.419127261608858,4.26432734830583));
#23884=CARTESIAN_POINT('Ctrl Pts',(22.736405157755,0.241238408088568,4.43283588997321));
#23885=CARTESIAN_POINT('Ctrl Pts',(22.7602630757865,0.00434171083240793,
4.49549632518638));
#23886=CARTESIAN_POINT('Ctrl Pts',(22.7841209938178,-0.233581370990537,
4.43700954435219));
#23887=CARTESIAN_POINT('Ctrl Pts',(22.8079789118493,-0.414457183229959,
4.27163232278894));
#23888=CARTESIAN_POINT('Ctrl Pts',(22.8238841905369,-0.46737397936094,4.11714349286348));
#23889=CARTESIAN_POINT('Ctrl Pts',(22.8318368298807,-0.473742730682552,
4.03823705100924));
#23890=CARTESIAN_POINT('Ctrl Pts',(4.,-0.219892372743211,3.64701365460636));
#23891=CARTESIAN_POINT('Ctrl Pts',(4.00795263934381,-0.161099076858729,
3.61038844940468));
#23892=CARTESIAN_POINT('Ctrl Pts',(4.02385791803142,-0.0249198690254346,
3.56711791692558));
#23893=CARTESIAN_POINT('Ctrl Pts',(4.04771583606284,0.185569069288609,3.60813812632505));
#23894=CARTESIAN_POINT('Ctrl Pts',(4.07157375409426,0.350624105231944,3.74494568050885));
#23895=CARTESIAN_POINT('Ctrl Pts',(4.09543167212568,0.429971014252744,3.94413788601839));
#23896=CARTESIAN_POINT('Ctrl Pts',(4.1192895901571,0.40416308778273,4.15698104289539));
#23897=CARTESIAN_POINT('Ctrl Pts',(4.14314750818851,0.279534313346206,4.3314427366163));
#23898=CARTESIAN_POINT('Ctrl Pts',(4.16700542621994,0.0865475313004802,
4.42485517705098));
#23899=CARTESIAN_POINT('Ctrl Pts',(4.19086334425134,-0.127600227202394,
4.41438026490915));
#23900=CARTESIAN_POINT('Ctrl Pts',(4.21472126228278,-0.310547447266788,
4.30257739619942));
#23901=CARTESIAN_POINT('Ctrl Pts',(4.23857918031418,-0.417556725585918,
4.11678647978038));
#23902=CARTESIAN_POINT('Ctrl Pts',(4.26243709834561,-0.422462345057068,
3.90243789311793));
#23903=CARTESIAN_POINT('Ctrl Pts',(4.28629501637703,-0.324064236326554,
3.71194600226016));
#23904=CARTESIAN_POINT('Ctrl Pts',(4.31015293440845,-0.146423688323203,
3.59189110566319));
#23905=CARTESIAN_POINT('Ctrl Pts',(4.33401085243986,0.0670214896752265,
3.5716299793216));
#23906=CARTESIAN_POINT('Ctrl Pts',(4.35786877047129,0.264078061498623,3.65611697628114));
#23907=CARTESIAN_POINT('Ctrl Pts',(4.38172668850271,0.396560367883193,3.82469274783887));
#23908=CARTESIAN_POINT('Ctrl Pts',(4.40558460653412,0.432072854850341,4.03613591352675));
#23909=CARTESIAN_POINT('Ctrl Pts',(4.42944252456555,0.361931763288092,4.23874286631049));
#23910=CARTESIAN_POINT('Ctrl Pts',(4.45330044259696,0.203288494707987,4.382970683851));
#23911=CARTESIAN_POINT('Ctrl Pts',(4.47715836062838,-0.00506434719902249,
4.43355173791626));
#23912=CARTESIAN_POINT('Ctrl Pts',(4.5010162786598,-0.212178818846594,4.37811758201071));
#23913=CARTESIAN_POINT('Ctrl Pts',(4.52487419669122,-0.367409789343613,
4.23022337776645));
#23914=CARTESIAN_POINT('Ctrl Pts',(4.54873211472264,-0.432799058467291,
4.02603328640456));
#23915=CARTESIAN_POINT('Ctrl Pts',(4.57259003275406,-0.392357168499796,
3.8154773474345));
#23916=CARTESIAN_POINT('Ctrl Pts',(4.59644795078547,-0.255973263285106,
3.65004222328625));
#23917=CARTESIAN_POINT('Ctrl Pts',(4.6203058688169,-0.0569969226013119,
3.57018130821703));
#23918=CARTESIAN_POINT('Ctrl Pts',(4.64416378684831,0.155916718210686,3.59542277130738));
#23919=CARTESIAN_POINT('Ctrl Pts',(4.66802170487973,0.330704474340828,3.71959438727947));
#23920=CARTESIAN_POINT('Ctrl Pts',(4.69187962291115,0.424625978282027,3.91233281365517));
#23921=CARTESIAN_POINT('Ctrl Pts',(4.71573754094257,0.41471486395576,4.1265082550995));
#23922=CARTESIAN_POINT('Ctrl Pts',(4.73959545897399,0.303394668785218,4.30974898215573));
#23923=CARTESIAN_POINT('Ctrl Pts',(4.76345337700541,0.117886212792376,4.41724764568232));
#23924=CARTESIAN_POINT('Ctrl Pts',(4.78731129503683,-0.0964486333844469,
4.42271789424177));
#23925=CARTESIAN_POINT('Ctrl Pts',(4.81116921306824,-0.287199161490599,
4.32482210305491));
#23926=CARTESIAN_POINT('Ctrl Pts',(4.83502713109967,-0.407721671464292,
4.14749845969467));
#23927=CARTESIAN_POINT('Ctrl Pts',(4.85888504913109,-0.42854512664958,3.93410742516172));
#23928=CARTESIAN_POINT('Ctrl Pts',(4.8827429671625,-0.344577625034195,3.73682892005441));
#23929=CARTESIAN_POINT('Ctrl Pts',(4.90660088519393,-0.176351507991885,
3.60390291263011));
#23930=CARTESIAN_POINT('Ctrl Pts',(4.93045880322534,0.0349973564730633,
3.56783343253575));
#23931=CARTESIAN_POINT('Ctrl Pts',(4.95431672125677,0.237788413971502,3.63744045016736));
#23932=CARTESIAN_POINT('Ctrl Pts',(4.97817463928818,0.382433727027559,3.79570315365689));
#23933=CARTESIAN_POINT('Ctrl Pts',(5.0020325573196,0.433563576539811,4.00392200101168));
#23934=CARTESIAN_POINT('Ctrl Pts',(5.02589047535102,0.378675321553375,4.21118181228595));
#23935=CARTESIAN_POINT('Ctrl Pts',(5.04974839338244,0.231190635538481,4.36680191797922));
#23936=CARTESIAN_POINT('Ctrl Pts',(5.07360631141386,0.0271735416279573,
4.43272896324296));
#23937=CARTESIAN_POINT('Ctrl Pts',(5.09746422944527,-0.183488223403015,
4.39284198969348));
#23938=CARTESIAN_POINT('Ctrl Pts',(5.1213221474767,-0.349282119693095,4.256894448863));
#23939=CARTESIAN_POINT('Ctrl Pts',(5.1451800655081,-0.4296670234643,4.05812921762123));
#23940=CARTESIAN_POINT('Ctrl Pts',(5.16903798353954,-0.404986636103755,
3.84514980926298));
#23941=CARTESIAN_POINT('Ctrl Pts',(5.19289590157095,-0.281275984601366,
3.67003549057442));
#23942=CARTESIAN_POINT('Ctrl Pts',(5.21675381960238,-0.0887856930599551,
3.5756064824932));
#23943=CARTESIAN_POINT('Ctrl Pts',(5.24061173763379,0.125415118908336,3.58495324968971));
#23944=CARTESIAN_POINT('Ctrl Pts',(5.26446965566521,0.308948518064291,3.69579025298356));
#23945=CARTESIAN_POINT('Ctrl Pts',(5.28832757369662,0.416935588964862,3.88101482593007));
#23946=CARTESIAN_POINT('Ctrl Pts',(5.31218549172805,0.422970551266107,4.09533451502773));
#23947=CARTESIAN_POINT('Ctrl Pts',(5.33604340975946,0.325577692296299,4.28634231834109));
#23948=CARTESIAN_POINT('Ctrl Pts',(5.35990132779089,0.148572219001774,4.40733162501188));
#23949=CARTESIAN_POINT('Ctrl Pts',(5.3837592458223,-0.0647632088646815,
4.42871725387658));
#23950=CARTESIAN_POINT('Ctrl Pts',(5.40761716385372,-0.26226226804932,4.34526983614494));
#23951=CARTESIAN_POINT('Ctrl Pts',(5.43147508188515,-0.395631058815178,
4.17739453851434));
#23952=CARTESIAN_POINT('Ctrl Pts',(5.45533299991656,-0.432257278927009,
3.96614144408682));
#23953=CARTESIAN_POINT('Ctrl Pts',(5.47919091794798,-0.363184819889405,
3.76316768886851));
#23954=CARTESIAN_POINT('Ctrl Pts',(5.5030488359794,-0.205303779432806,3.61810588490468));
#23955=CARTESIAN_POINT('Ctrl Pts',(5.52690675401082,0.00277962745745752,
3.56642759466814));
#23956=CARTESIAN_POINT('Ctrl Pts',(5.55076467204224,0.210183339719457,3.62076956781107));
#23957=CARTESIAN_POINT('Ctrl Pts',(5.57462259007365,0.36619150013966,3.76784371165257));
#23958=CARTESIAN_POINT('Ctrl Pts',(5.59848050810508,0.432655863921731,3.97168639180759));
#23959=CARTESIAN_POINT('Ctrl Pts',(5.62233842613649,0.393324083661671,4.18245252040861));
#23960=CARTESIAN_POINT('Ctrl Pts',(5.64619634416792,0.257813851021257,4.34860403787086));
#23961=CARTESIAN_POINT('Ctrl Pts',(5.67005426219933,0.0592611090830247,
4.42951237227525));
#23962=CARTESIAN_POINT('Ctrl Pts',(5.69391218023075,-0.153782588238227,
4.40539323200473));
#23963=CARTESIAN_POINT('Ctrl Pts',(5.71777009826218,-0.329222253834466,
4.28214440376531));
#23964=CARTESIAN_POINT('Ctrl Pts',(5.74162801629359,-0.424158110434281,
4.08990358344764));
#23965=CARTESIAN_POINT('Ctrl Pts',(5.76548593432501,-0.415375755386326,
3.8756788878607));
#23966=CARTESIAN_POINT('Ctrl Pts',(5.78934385235642,-0.305022713182347,
3.69185409099321));
#23967=CARTESIAN_POINT('Ctrl Pts',(5.81320177038785,-0.120083309624962,
3.58337936191985));
#23968=CARTESIAN_POINT('Ctrl Pts',(5.83705968841926,0.0942197354074567,
3.57677972866706));
#23969=CARTESIAN_POINT('Ctrl Pts',(5.86091760645069,0.285483486244351,3.673668977605));
#23970=CARTESIAN_POINT('Ctrl Pts',(5.8847755244821,0.406938752801468,3.85035505520226));
#23971=CARTESIAN_POINT('Ctrl Pts',(5.90863344251353,0.428886400972996,4.06363338935351));
#23972=CARTESIAN_POINT('Ctrl Pts',(5.93249136054494,0.345959657594393,4.261351642888));
#23973=CARTESIAN_POINT('Ctrl Pts',(5.95634927857636,0.178436323746589,4.39516226965834));
#23974=CARTESIAN_POINT('Ctrl Pts',(5.98020719660778,-0.0327194942966983,
4.4323450160316));
#23975=CARTESIAN_POINT('Ctrl Pts',(6.0040651146392,-0.23587461323539,4.36380751861078));
#23976=CARTESIAN_POINT('Ctrl Pts',(6.02792303267061,-0.381351759249696,
4.20630938167977));
#23977=CARTESIAN_POINT('Ctrl Pts',(6.05178095070204,-0.433578399193506,
3.9983625870902));
#23978=CARTESIAN_POINT('Ctrl Pts',(6.07563886873346,-0.379782579589031,
3.79081692866841));
#23979=CARTESIAN_POINT('Ctrl Pts',(6.09949678676487,-0.233120953551068,
3.63442082419035));
#23980=CARTESIAN_POINT('Ctrl Pts',(6.12335470479629,-0.0294522997972467,
3.5674214393556));
#23981=CARTESIAN_POINT('Ctrl Pts',(6.14721262282771,0.181413325723775,3.60619428643423));
#23982=CARTESIAN_POINT('Ctrl Pts',(6.17107054085913,0.347927737305898,3.74127281623538));
#23983=CARTESIAN_POINT('Ctrl Pts',(6.19492845889055,0.429346806292137,3.93959933010928));
#23984=CARTESIAN_POINT('Ctrl Pts',(6.21878637692197,0.405811992579865,4.15272917617017));
#23985=CARTESIAN_POINT('Ctrl Pts',(6.24264429495339,0.282982581651336,4.32844890303245));
#23986=CARTESIAN_POINT('Ctrl Pts',(6.26650221298481,0.0910742457207041,
4.42397415233781));
#23987=CARTESIAN_POINT('Ctrl Pts',(6.29036013101623,-0.123327005978964,
4.41559921078967));
#23988=CARTESIAN_POINT('Ctrl Pts',(6.31421804904765,-0.307151379675736,
4.3060270879454));
#23989=CARTESIAN_POINT('Ctrl Pts',(6.33807596707907,-0.416657206472865,
4.12081787696614));
#23990=CARTESIAN_POINT('Ctrl Pts',(6.36193388511048,-0.422829889105799,
3.9075587958503));
#23991=CARTESIAN_POINT('Ctrl Pts',(6.39374444248571,-0.296437506874183,
3.64987069373525));
#23992=CARTESIAN_POINT('Ctrl Pts',(6.43350763920474,0.0703302468340302,
3.51324810367198));
#23993=CARTESIAN_POINT('Ctrl Pts',(6.48122347526758,0.448014600657906,3.7964368525222));
#23994=CARTESIAN_POINT('Ctrl Pts',(6.52893931133042,0.413240052911115,4.26646358767058));
#23995=CARTESIAN_POINT('Ctrl Pts',(6.57665514739325,-0.000480251589724132,
4.49184654025612));
#23996=CARTESIAN_POINT('Ctrl Pts',(6.62437098345609,-0.41404349770976,4.26553045144514));
#23997=CARTESIAN_POINT('Ctrl Pts',(6.67208681951894,-0.447234019333667,
3.79538894860702));
#23998=CARTESIAN_POINT('Ctrl Pts',(6.71980265558177,-0.0698021891909718,
3.51313682319347));
#23999=CARTESIAN_POINT('Ctrl Pts',(6.76751849164461,0.371772181936036,3.67798293440124));
#24000=CARTESIAN_POINT('Ctrl Pts',(6.81523432770745,0.471920133146607,4.13853999974893));
#24001=CARTESIAN_POINT('Ctrl Pts',(6.86295016377028,0.138708377331583,4.4718748549198));
#24002=CARTESIAN_POINT('Ctrl Pts',(6.91066599983312,-0.32188767172048,4.37187913281409));
#24003=CARTESIAN_POINT('Ctrl Pts',(6.95838183589596,-0.486886005735063,
3.93038141845316));
#24004=CARTESIAN_POINT('Ctrl Pts',(7.0060976719588,-0.204771183672361,3.55281534000283));
#24005=CARTESIAN_POINT('Ctrl Pts',(7.05381350802163,0.265389096458903,3.58590591031157));
#24006=CARTESIAN_POINT('Ctrl Pts',(7.10152934408448,0.491837993618785,3.99926540470374));
#24007=CARTESIAN_POINT('Ctrl Pts',(7.14924518014731,0.266624753986561,4.41329951581085));
#24008=CARTESIAN_POINT('Ctrl Pts',(7.19696101621015,-0.203434237821079,
4.44779430805676));
#24009=CARTESIAN_POINT('Ctrl Pts',(7.24467685227299,-0.486676365692783,
4.07107270446015));
#24010=CARTESIAN_POINT('Ctrl Pts',(7.29239268833582,-0.322996137187983,
3.62908393881966));
#24011=CARTESIAN_POINT('Ctrl Pts',(7.34010852439867,0.137296434535941,3.52771310152703));
#24012=CARTESIAN_POINT('Ctrl Pts',(7.3878243604615,0.471507566988788,3.86005058906394));
#24013=CARTESIAN_POINT('Ctrl Pts',(7.43554019652434,0.372726051350611,4.32090577464778));
#24014=CARTESIAN_POINT('Ctrl Pts',(7.48325603258718,-0.0683355354161961,
4.48706824929225));
#24015=CARTESIAN_POINT('Ctrl Pts',(7.53097186865002,-0.44664354691983,4.20594845626764));
#24016=CARTESIAN_POINT('Ctrl Pts',(7.57868770471286,-0.414791917646955,
3.73570302684109));
#24017=CARTESIAN_POINT('Ctrl Pts',(7.62640354077569,-0.00203048755240202,
3.50816557464413));
#24018=CARTESIAN_POINT('Ctrl Pts',(7.67411937683853,0.412595570264971,3.73228724307244));
#24019=CARTESIAN_POINT('Ctrl Pts',(7.72183521290137,0.448328767436039,4.20225365549051));
#24020=CARTESIAN_POINT('Ctrl Pts',(7.7695510489642,0.0723547589785895,4.48648742399228));
#24021=CARTESIAN_POINT('Ctrl Pts',(7.81726688502705,-0.370063737934377,
4.32397230547438));
#24022=CARTESIAN_POINT('Ctrl Pts',(7.86498272108989,-0.472647010158531,
3.86394843388276));
#24023=CARTESIAN_POINT('Ctrl Pts',(7.91269855715272,-0.141191260335066,
3.52886280888004));
#24024=CARTESIAN_POINT('Ctrl Pts',(7.96041439321556,0.31992259635559,3.62642971585976));
#24025=CARTESIAN_POINT('Ctrl Pts',(8.0081302292784,0.48724661017382,4.0670519628834));
#24026=CARTESIAN_POINT('Ctrl Pts',(8.05584606534124,0.207124564615173,4.44609936066402));
#24027=CARTESIAN_POINT('Ctrl Pts',(8.10356190140407,-0.263203155649882,
4.41548685142597));
#24028=CARTESIAN_POINT('Ctrl Pts',(8.15127773746691,-0.491827368180951,
4.00332637343646));
#24029=CARTESIAN_POINT('Ctrl Pts',(8.19899357352975,-0.268798940774433,
3.58811123553743));
#24030=CARTESIAN_POINT('Ctrl Pts',(8.24670940959259,0.201071689948468,3.55113988776764));
#24031=CARTESIAN_POINT('Ctrl Pts',(8.29442524565542,0.486295093906121,3.92636368766143));
#24032=CARTESIAN_POINT('Ctrl Pts',(8.34214108171827,0.324946230517931,4.36920884621601));
#24033=CARTESIAN_POINT('Ctrl Pts',(8.3898569177811,-0.134805756295296,4.47300384028212));
#24034=CARTESIAN_POINT('Ctrl Pts',(8.43757275384394,-0.470763542849379,
4.14243212971755));
#24035=CARTESIAN_POINT('Ctrl Pts',(8.48528858990678,-0.37441192437669,3.68106280283335));
#24036=CARTESIAN_POINT('Ctrl Pts',(8.53300442596962,0.0657679253190804,
3.51257841158684));
#24037=CARTESIAN_POINT('Ctrl Pts',(8.58072026203246,0.445552077224736,3.79170076492532));
#24038=CARTESIAN_POINT('Ctrl Pts',(8.62843609809529,0.41617890091499,4.26210751092856));
#24039=CARTESIAN_POINT('Ctrl Pts',(8.67615193415813,0.0046222361594965,
4.49181689660367));
#24040=CARTESIAN_POINT('Ctrl Pts',(8.72386777022097,-0.411179099183508,
4.26988325855195));
#24041=CARTESIAN_POINT('Ctrl Pts',(8.7715836062838,-0.449388340942622,3.80011167148426));
#24042=CARTESIAN_POINT('Ctrl Pts',(8.81929944234665,-0.0749173544856965,
3.51390061216986));
#24043=CARTESIAN_POINT('Ctrl Pts',(8.86701527840948,0.368351391347115,3.67408210030036));
#24044=CARTESIAN_POINT('Ctrl Pts',(8.91473111447233,0.473357386691186,4.13355901061654));
#24045=CARTESIAN_POINT('Ctrl Pts',(8.96244695053515,0.14367201029714,4.47038662641401));
#24046=CARTESIAN_POINT('Ctrl Pts',(9.01016278659801,-0.317949583830803,
4.37525096534692));
#24047=CARTESIAN_POINT('Ctrl Pts',(9.05787862266083,-0.487593182843731,
3.93551656882348));
#24048=CARTESIAN_POINT('Ctrl Pts',(9.10559445872368,-0.209472459465777,
3.55499829935456));
#24049=CARTESIAN_POINT('Ctrl Pts',(9.15331029478651,0.261010046587687,3.58313193881964));
#24050=CARTESIAN_POINT('Ctrl Pts',(9.20102613084934,0.491803010703882,3.99408193320625));
#24051=CARTESIAN_POINT('Ctrl Pts',(9.2487419669122,0.270965702728691,4.41046657939073));
#24052=CARTESIAN_POINT('Ctrl Pts',(9.29645780297501,-0.198703579405513,
4.44991344988054));
#24053=CARTESIAN_POINT('Ctrl Pts',(9.34417363903789,-0.485900307124067,
4.07619787653679));
#24054=CARTESIAN_POINT('Ctrl Pts',(9.39188947510068,-0.326887306273347,
3.63250862071426));
#24055=CARTESIAN_POINT('Ctrl Pts',(9.43960531116356,0.13231133773591,3.52629235307153));
#24056=CARTESIAN_POINT('Ctrl Pts',(9.48732114722637,0.470006444430667,3.85508910653225));
#24057=CARTESIAN_POINT('Ctrl Pts',(9.53503698328922,0.376087401226012,4.31695976320512));
#24058=CARTESIAN_POINT('Ctrl Pts',(9.58275281935206,-0.0631984893729827,
4.48776139227388));
#24059=CARTESIAN_POINT('Ctrl Pts',(9.63046865541489,-0.444448234747017,
4.21064422964382));
#24060=CARTESIAN_POINT('Ctrl Pts',(9.67818449147773,-0.41755432743774,3.74008922975375));
#24061=CARTESIAN_POINT('Ctrl Pts',(9.72590032754057,-0.00721385634321597,
3.50821428942208));
#24062=CARTESIAN_POINT('Ctrl Pts',(9.77361616360341,0.40975121003073,3.72795373420991));
#24063=CARTESIAN_POINT('Ctrl Pts',(9.82133199966624,0.450435435400681,4.19751745084266));
#24064=CARTESIAN_POINT('Ctrl Pts',(9.86904783572909,0.077477869602138,4.48569785316993));
#24065=CARTESIAN_POINT('Ctrl Pts',(9.91676367179192,-0.366628816002305,
4.3278544435092));
#24066=CARTESIAN_POINT('Ctrl Pts',(9.96447950785476,-0.474054618562381,
3.8689372536849));
#24067=CARTESIAN_POINT('Ctrl Pts',(10.0121953439176,-0.146148770628728,
3.53037700046135));
#24068=CARTESIAN_POINT('Ctrl Pts',(10.0599111799804,0.315967742161179,3.62307877379278));
#24069=CARTESIAN_POINT('Ctrl Pts',(10.1076270160433,0.487926215535836,4.06191310882887));
#24070=CARTESIAN_POINT('Ctrl Pts',(10.1553428521061,0.211814537474087,4.44389168337175));
#24071=CARTESIAN_POINT('Ctrl Pts',(10.203058688169,-0.258809689535701,4.4182376949229));
#24072=CARTESIAN_POINT('Ctrl Pts',(10.2507745242318,-0.491764996345908,
4.00850959581219));
#24073=CARTESIAN_POINT('Ctrl Pts',(10.2984903602946,-0.273124940234581,
3.59096700393021));
#24074=CARTESIAN_POINT('Ctrl Pts',(10.3462061963575,0.196329951061554,3.54904570612073));
#24075=CARTESIAN_POINT('Ctrl Pts',(10.3939220324203,0.485492027373267,3.92124267520431));
#24076=CARTESIAN_POINT('Ctrl Pts',(10.4416378684831,0.328819304693055,4.36576370748498));
#24077=CARTESIAN_POINT('Ctrl Pts',(10.489353704546,-0.129813245022134,4.47439829918413));
#24078=CARTESIAN_POINT('Ctrl Pts',(10.5370695406088,-0.469236294399976,
4.14738563318641));
#24079=CARTESIAN_POINT('Ctrl Pts',(10.5847853766716,-0.377752434501872,
3.68502647241413));
#24080=CARTESIAN_POINT('Ctrl Pts',(10.6325012127345,0.0606272984676223,
3.51191234851464));
#24081=CARTESIAN_POINT('Ctrl Pts',(10.6802170487973,0.443332050383407,3.78701662516801));
#24082=CARTESIAN_POINT('Ctrl Pts',(10.7279328848602,0.418918158891686,4.25770681210006));
#24083=CARTESIAN_POINT('Ctrl Pts',(10.775648720923,0.00980527620531799,
4.49174086815163));
#24084=CARTESIAN_POINT('Ctrl Pts',(10.8233645569858,-0.408311942493964,
4.27420171857372));
#24085=CARTESIAN_POINT('Ctrl Pts',(10.8710803930487,-0.451470021714238,
3.80485891169382));
#24086=CARTESIAN_POINT('Ctrl Pts',(10.9187962291115,-0.080036233235122,
3.51471716883706));
#24087=CARTESIAN_POINT('Ctrl Pts',(10.9665120651743,0.364896059739551,3.6702181168734));
#24088=CARTESIAN_POINT('Ctrl Pts',(11.0142279012372,0.47473868640782,4.1285628425314));
#24089=CARTESIAN_POINT('Ctrl Pts',(11.0619437373,0.148621472554162,4.46884633169921));
#24090=CARTESIAN_POINT('Ctrl Pts',(11.1096595733629,-0.313977126381285,
4.37858102033954));
#24091=CARTESIAN_POINT('Ctrl Pts',(11.1573754094257,-0.488245699001722,
3.94065893278431));
#24092=CARTESIAN_POINT('Ctrl Pts',(11.2050912454886,-0.214150733603143,
3.55723066033293));
#24093=CARTESIAN_POINT('Ctrl Pts',(11.2528070815514,0.256602145595791,3.58040428537983));
#24094=CARTESIAN_POINT('Ctrl Pts',(11.3005229176142,0.491713326162588,3.98889911147238));
#24095=CARTESIAN_POINT('Ctrl Pts',(11.3482387536771,0.275276593332242,4.40758805430897));
#24096=CARTESIAN_POINT('Ctrl Pts',(11.3959545897399,-0.193950870829933,
4.45198261532529));
#24097=CARTESIAN_POINT('Ctrl Pts',(11.4436704258028,-0.485070265991237,
4.08131458604192));
#24098=CARTESIAN_POINT('Ctrl Pts',(11.4913862618656,-0.330742172127369,
3.63597412121053));
#24099=CARTESIAN_POINT('Ctrl Pts',(11.5391020979284,0.127311547523522,3.52492422212962));
#24100=CARTESIAN_POINT('Ctrl Pts',(11.5868179339912,0.468453114143607,3.85014371984754));
#24101=CARTESIAN_POINT('Ctrl Pts',(11.6345337700541,0.379406977967949,4.31297854546471));
#24102=CARTESIAN_POINT('Ctrl Pts',(11.6822496061169,-0.0580544240024287,
4.48840035698771));
#24103=CARTESIAN_POINT('Ctrl Pts',(11.7299654421798,-0.44220355512924,4.21531660568344));
#24104=CARTESIAN_POINT('Ctrl Pts',(11.7776812782426,-0.420270357404582,
3.74450430230823));
#24105=CARTESIAN_POINT('Ctrl Pts',(11.8253971143054,-0.0123964237846327,
3.50831762943));
#24106=CARTESIAN_POINT('Ctrl Pts',(11.8731129503683,0.406861336540243,3.72365044295193));
#24107=CARTESIAN_POINT('Ctrl Pts',(11.9208287864311,0.452492071153857,4.1927593068956));
#24108=CARTESIAN_POINT('Ctrl Pts',(11.968544622494,0.0825923743414284,4.48485433333386));
#24109=CARTESIAN_POINT('Ctrl Pts',(12.0162604585568,-0.363153170675764,
4.33170016502878));
#24110=CARTESIAN_POINT('Ctrl Pts',(12.0639762946196,-0.475409571231627,
3.87394063131468));
#24111=CARTESIAN_POINT('Ctrl Pts',(12.1116921306825,-0.151090047408964,
3.53194335553704));
#24112=CARTESIAN_POINT('Ctrl Pts',(12.1594079667453,0.311977791768556,3.61976969834691));
#24113=CARTESIAN_POINT('Ctrl Pts',(12.2071238028081,0.488551624369653,4.05676737776005));
#24114=CARTESIAN_POINT('Ctrl Pts',(12.254839638871,0.216480982979095,4.44163470069774));
#24115=CARTESIAN_POINT('Ctrl Pts',(12.3025554749338,-0.254387476069249,
4.42094208256136));
#24116=CARTESIAN_POINT('Ctrl Pts',(12.3502713109967,-0.49164800158875,4.0136918729824));
#24117=CARTESIAN_POINT('Ctrl Pts',(12.3979871470595,-0.277420602272412,
3.59386820576715));
#24118=CARTESIAN_POINT('Ctrl Pts',(12.4457029831224,0.191566404775332,3.54700161433684));
#24119=CARTESIAN_POINT('Ctrl Pts',(12.4934188191852,0.484635034689867,3.91613041073711));
#24120=CARTESIAN_POINT('Ctrl Pts',(12.541134655248,0.332655855180181,4.362277941457));
#24121=CARTESIAN_POINT('Ctrl Pts',(12.5888504913109,-0.124806314709729,
4.47574006417428));
#24122=CARTESIAN_POINT('Ctrl Pts',(12.6365663273737,-0.4676569254097,4.15232276575852));
#24123=CARTESIAN_POINT('Ctrl Pts',(12.6842821634365,-0.381050985679211,
3.68902512775968));
#24124=CARTESIAN_POINT('Ctrl Pts',(12.7319979994994,0.0554799374235607,
3.5113004999026));
#24125=CARTESIAN_POINT('Ctrl Pts',(12.7797138355622,0.441062780321708,3.78235614259331));
#24126=CARTESIAN_POINT('Ctrl Pts',(12.8274296716251,0.421610885427219,4.2532774884218));
#24127=CARTESIAN_POINT('Ctrl Pts',(12.8751455076879,0.0149872271275763,
4.49161021945745));
#24128=CARTESIAN_POINT('Ctrl Pts',(12.9228613437507,-0.405399432451448,
4.27848972156979));
#24129=CARTESIAN_POINT('Ctrl Pts',(12.9705771798136,-0.453501555338242,
3.80962782724943));
#24130=CARTESIAN_POINT('Ctrl Pts',(13.0182930158764,-0.0851462219395619,
3.51558762841831));
#24131=CARTESIAN_POINT('Ctrl Pts',(13.0660088519392,0.361400197209248,3.66639076405307));
#24132=CARTESIAN_POINT('Ctrl Pts',(13.1137246880021,0.476067254403989,4.1235523942958));
#24133=CARTESIAN_POINT('Ctrl Pts',(13.1614405240649,0.153554426643267,4.46725395975876));
#24134=CARTESIAN_POINT('Ctrl Pts',(13.2091563601278,-0.30996979384252,4.38186902434892));
#24135=CARTESIAN_POINT('Ctrl Pts',(13.2568721961906,-0.488843983144383,
3.94580788806928));
#24136=CARTESIAN_POINT('Ctrl Pts',(13.3045880322534,-0.218805220893238,
3.55951220202843));
#24137=CARTESIAN_POINT('Ctrl Pts',(13.3523038683163,0.252165742455243,3.57772323864086));
#24138=CARTESIAN_POINT('Ctrl Pts',(13.4000197043791,0.491569024438394,3.98371752277252));
#24139=CARTESIAN_POINT('Ctrl Pts',(13.447735540442,0.279556907518101,4.40466425628032));
#24140=CARTESIAN_POINT('Ctrl Pts',(13.4954513765048,-0.189176619112,4.45400157668594));
#24141=CARTESIAN_POINT('Ctrl Pts',(13.5431672125676,-0.484186345555107,
4.08642226350871));
#24142=CARTESIAN_POINT('Ctrl Pts',(13.5908830486304,-0.334560300710407,
3.63948005597396));
#24143=CARTESIAN_POINT('Ctrl Pts',(13.6385988846933,0.122297616148583,3.52360886035071));
#24144=CARTESIAN_POINT('Ctrl Pts',(13.6863147207561,0.466847750307624,3.8452149784873));
#24145=CARTESIAN_POINT('Ctrl Pts',(13.734030556819,0.3826844119832,4.30896256355269));
#24146=CARTESIAN_POINT('Ctrl Pts',(13.7817463928818,-0.0529039102219543,
4.48898507250754));
#24147=CARTESIAN_POINT('Ctrl Pts',(13.8294622289446,-0.439909757638992,
4.21996506537626));
#24148=CARTESIAN_POINT('Ctrl Pts',(13.8771780650075,-0.422939705734467,
3.74894775411238));
#24149=CARTESIAN_POINT('Ctrl Pts',(13.9248939010703,-0.0175776142901187,
3.50847558318244));
#24150=CARTESIAN_POINT('Ctrl Pts',(13.9726097371332,0.403926270823208,3.71937784729135));
#24151=CARTESIAN_POINT('Ctrl Pts',(14.020325573196,0.454498446235019,4.18797975215946));
#24152=CARTESIAN_POINT('Ctrl Pts',(14.0680414092588,0.0876977051117048,
4.48395695817926));
#24153=CARTESIAN_POINT('Ctrl Pts',(14.1157572453217,-0.359637188018331,
4.33550904286807));
#24154=CARTESIAN_POINT('Ctrl Pts',(14.1634730813845,-0.476711717661702,
3.87895801102093));
#24155=CARTESIAN_POINT('Ctrl Pts',(14.2111889174473,-0.156014541823709,
3.53356170012368));
#24156=CARTESIAN_POINT('Ctrl Pts',(14.2589047535102,0.307953188363286,3.61650285707861));
#24157=CARTESIAN_POINT('Ctrl Pts',(14.306620589573,0.4891227672074,4.05161534124029));
#24158=CARTESIAN_POINT('Ctrl Pts',(14.3543364256359,0.2211233828038,4.4393286633369));
#24159=CARTESIAN_POINT('Ctrl Pts',(14.4020522616987,-0.249937006449114,
4.42359971395084));
#24160=CARTESIAN_POINT('Ctrl Pts',(14.4497680977616,-0.491476396904638,
4.01887262932433));
#24161=CARTESIAN_POINT('Ctrl Pts',(14.4974839338244,-0.281685449746218,
3.59681451879656));
#24162=CARTESIAN_POINT('Ctrl Pts',(14.5451997698872,0.186781580201919,3.54500783946397));
#24163=CARTESIAN_POINT('Ctrl Pts',(14.59291560595,0.483724211046603,3.91102746210588));
#24164=CARTESIAN_POINT('Ctrl Pts',(14.6406314420129,0.33645545583349,4.35875193531444));
#24165=CARTESIAN_POINT('Ctrl Pts',(14.6883472780757,-0.119785521504147,
4.47702898621568));
#24166=CARTESIAN_POINT('Ctrl Pts',(14.7360631141386,-0.466025611307368,
4.15724297904063));
#24167=CARTESIAN_POINT('Ctrl Pts',(14.7837789502014,-0.38430721152129,3.69305832471834));
#24168=CARTESIAN_POINT('Ctrl Pts',(14.8314947862642,0.0503264139313189,
3.51074293371195));
#24169=CARTESIAN_POINT('Ctrl Pts',(14.8792106223271,0.438744519099385,3.77771983486548));
#24170=CARTESIAN_POINT('Ctrl Pts',(14.9269264583899,0.42425678142631,4.24882003188202));
#24171=CARTESIAN_POINT('Ctrl Pts',(14.9746422944528,0.0201675133397715,
4.49142496503298));
#24172=CARTESIAN_POINT('Ctrl Pts',(15.0223581305156,-0.402441892563756,
4.28274679124913));
#24173=CARTESIAN_POINT('Ctrl Pts',(15.0700739665785,-0.455482716161518,
3.8144178884426));
#24174=CARTESIAN_POINT('Ctrl Pts',(15.1177898026413,-0.0902467530057116,
3.51651189422706));
#24175=CARTESIAN_POINT('Ctrl Pts',(15.1655056387041,0.357864192060027,3.66260046696357));
#24176=CARTESIAN_POINT('Ctrl Pts',(15.2132214747669,0.47734294310866,4.11852822244656));
#24177=CARTESIAN_POINT('Ctrl Pts',(15.2609373108298,0.15847032463534,4.46560968746574));
#24178=CARTESIAN_POINT('Ctrl Pts',(15.3086531468926,-0.305928031329979,
4.38511461215921));
#24179=CARTESIAN_POINT('Ctrl Pts',(15.3563689829555,-0.489387968817152,
3.95096286275689));
#24180=CARTESIAN_POINT('Ctrl Pts',(15.4040848190183,-0.223435404337718,
3.56184267101825));
#24181=CARTESIAN_POINT('Ctrl Pts',(15.4518006550811,0.24770132994065,3.57508909640066));
#24182=CARTESIAN_POINT('Ctrl Pts',(15.499516491144,0.491370121559653,3.97853774265298));
#24183=CARTESIAN_POINT('Ctrl Pts',(15.5472323272068,0.283806169849271,4.40169551006635));
#24184=CARTESIAN_POINT('Ctrl Pts',(15.5949481632697,-0.184381354552937,
4.4559701097059));
#24185=CARTESIAN_POINT('Ctrl Pts',(15.6426639993325,-0.483248643997369,
4.09152034160055));
#24186=CARTESIAN_POINT('Ctrl Pts',(15.6903798353953,-0.338341267922855,
3.64302603558196));
#24187=CARTESIAN_POINT('Ctrl Pts',(15.7380956714582,0.117270100534806,3.52234641383892));
#24188=CARTESIAN_POINT('Ctrl Pts',(15.785811507521,0.465190531238913,3.84030342991275));
#24189=CARTESIAN_POINT('Ctrl Pts',(15.8335273435838,0.385919339229949,4.30491226354526));
#24190=CARTESIAN_POINT('Ctrl Pts',(15.8812431796467,-0.0477475201261761,
4.48951547388594));
#24191=CARTESIAN_POINT('Ctrl Pts',(15.9289590157095,-0.437567097060412,
4.22458909239344));
#24192=CARTESIAN_POINT('Ctrl Pts',(15.9766748517724,-0.425562075928853,
3.75341909160864));
#24193=CARTESIAN_POINT('Ctrl Pts',(16.0243906878352,-0.0227568523576073,
3.50868813313462));
#24194=CARTESIAN_POINT('Ctrl Pts',(16.072106523898,0.400946338892803,3.71513642180785));
#24195=CARTESIAN_POINT('Ctrl Pts',(16.1198223599609,0.456454337785543,4.1831793175245));
#24196=CARTESIAN_POINT('Ctrl Pts',(16.1675381960237,0.0927932948370443,
4.4830058273823));
#24197=CARTESIAN_POINT('Ctrl Pts',(16.2152540320865,-0.356081258568678,
4.33928065395499));
#24198=CARTESIAN_POINT('Ctrl Pts',(16.2629698681494,-0.477960913216358,
3.88398883549692));
#24199=CARTESIAN_POINT('Ctrl Pts',(16.3106857042122,-0.160921706883503,
3.53523185446324));
#24200=CARTESIAN_POINT('Ctrl Pts',(16.358401540275,0.303894378979202,3.6132786128531));
#24201=CARTESIAN_POINT('Ctrl Pts',(16.4061173763379,0.489639580609251,4.04645757153336));
#24202=CARTESIAN_POINT('Ctrl Pts',(16.4538332124007,0.225741221292456,4.43697382743292));
#24203=CARTESIAN_POINT('Ctrl Pts',(16.5015490484636,-0.245458775012363,
4.42621029389423));
#24204=CARTESIAN_POINT('Ctrl Pts',(16.5492648845264,-0.4912502013546,4.02405128938415));
#24205=CARTESIAN_POINT('Ctrl Pts',(16.5969807205893,-0.285919008936969,
3.59980561575594));
#24206=CARTESIAN_POINT('Ctrl Pts',(16.6446965566521,0.181976008816936,3.54306460296116));
#24207=CARTESIAN_POINT('Ctrl Pts',(16.6924123927149,0.482759657613431,3.90593439612197));
#24208=CARTESIAN_POINT('Ctrl Pts',(16.7401282287778,0.340217684611379,4.35518608070932));
#24209=CARTESIAN_POINT('Ctrl Pts',(16.7878440648406,-0.114751423091257,
4.47826492214097));
#24210=CARTESIAN_POINT('Ctrl Pts',(16.8355599009034,-0.464342533291602,
4.16214572651883));
#24211=CARTESIAN_POINT('Ctrl Pts',(16.8832757369663,-0.387520750342007,
3.69712561530174));
#24212=CARTESIAN_POINT('Ctrl Pts',(16.9309915730291,0.0451673004198413,
3.51023971187451));
#24213=CARTESIAN_POINT('Ctrl Pts',(16.978707409092,0.436377524217892,3.7731082169636));
#24214=CARTESIAN_POINT('Ctrl Pts',(17.0264232451548,0.426855552995382,4.24433493759383));
#24215=CARTESIAN_POINT('Ctrl Pts',(17.0741390812176,0.0253455594402812,
4.49118512545541));
#24216=CARTESIAN_POINT('Ctrl Pts',(17.1218549172805,-0.399439651340385,
4.28697245475663));
#24217=CARTESIAN_POINT('Ctrl Pts',(17.1695707533433,-0.457413284126125,
3.81922856321607));
#24218=CARTESIAN_POINT('Ctrl Pts',(17.2172865894061,-0.0953372598908034,
3.51748986360026));
#24219=CARTESIAN_POINT('Ctrl Pts',(17.265002425469,0.354288437054553,3.6588476466131));
#24220=CARTESIAN_POINT('Ctrl Pts',(17.3127182615318,0.478565610824392,4.11349088504481));
#24221=CARTESIAN_POINT('Ctrl Pts',(17.3604340975947,0.163368620495752,4.46391369745815));
#24222=CARTESIAN_POINT('Ctrl Pts',(17.4081499336575,-0.301852287783465,
4.38831742326589));
#24223=CARTESIAN_POINT('Ctrl Pts',(17.4558657697204,-0.489877595596684,
3.956123284257));
#24224=CARTESIAN_POINT('Ctrl Pts',(17.5035816057832,-0.228040769637767,
3.56422180844494));
#24225=CARTESIAN_POINT('Ctrl Pts',(17.551297441846,0.243209403937772,3.57250215124727));
#24226=CARTESIAN_POINT('Ctrl Pts',(17.5990132779089,0.491116639619549,3.97336034645914));
#24227=CARTESIAN_POINT('Ctrl Pts',(17.6467291139717,0.288023908337871,4.39868214542132));
#24228=CARTESIAN_POINT('Ctrl Pts',(17.6944449500345,-0.179565609787963,
4.45788799572981));
#24229=CARTESIAN_POINT('Ctrl Pts',(17.7421607860973,-0.48225726547346,4.09660825404716));
#24230=CARTESIAN_POINT('Ctrl Pts',(17.7898766221602,-0.342084653792828,
3.64661166616396));
#24231=CARTESIAN_POINT('Ctrl Pts',(17.837592458223,0.112229559114723,3.52113702282083));
#24232=CARTESIAN_POINT('Ctrl Pts',(17.8853082942859,0.463481641013499,3.83540961967535));
#24233=CARTESIAN_POINT('Ctrl Pts',(17.9330241303487,0.389111400387848,4.30082809533052));
#24234=CARTESIAN_POINT('Ctrl Pts',(17.9807399664116,-0.0425858264624495,
4.48999150220845));
#24235=CARTESIAN_POINT('Ctrl Pts',(18.0284558024744,-0.435175833605105,
4.22918817311999));
#24236=CARTESIAN_POINT('Ctrl Pts',(18.0761716385373,-0.428137176707308,
3.75791781814212));
#24237=CARTESIAN_POINT('Ctrl Pts',(18.1238874746,-0.0279335627019553,3.5089552556775));
#24238=CARTESIAN_POINT('Ctrl Pts',(18.1716033106629,0.397921871745719,3.71092663761881));
#24239=CARTESIAN_POINT('Ctrl Pts',(18.2193191467257,0.458359528554279,4.17835853620019));
#24240=CARTESIAN_POINT('Ctrl Pts',(18.2670349827886,0.097878577523561,4.48200104659009));
#24241=CARTESIAN_POINT('Ctrl Pts',(18.3147508188514,-0.352485777302551,
4.34301457935691));
#24242=CARTESIAN_POINT('Ctrl Pts',(18.3624666549143,-0.479157019140895,
3.88903254594255));
#24243=CARTESIAN_POINT('Ctrl Pts',(18.4101824909771,-0.165810997523729,
3.5369536330429));
#24244=CARTESIAN_POINT('Ctrl Pts',(18.4578983270399,0.299801814449608,3.61009732380414));
#24245=CARTESIAN_POINT('Ctrl Pts',(18.5056141631028,0.49010200717001,4.04129464153984));
#24246=CARTESIAN_POINT('Ctrl Pts',(18.5533299991656,0.230333985517487,4.43457045454981));
#24247=CARTESIAN_POINT('Ctrl Pts',(18.6010458352284,-0.24095327917969,4.42877353242069));
#24248=CARTESIAN_POINT('Ctrl Pts',(18.6487616712913,-0.49096944006335,4.0292272779409));
#24249=CARTESIAN_POINT('Ctrl Pts',(18.6964775073541,-0.290120809601049,
3.60284116440841));
#24250=CARTESIAN_POINT('Ctrl Pts',(18.744193343417,0.177150224400508,3.54117212067402));
#24251=CARTESIAN_POINT('Ctrl Pts',(18.7919091794797,0.481741481528227,3.90085177849878));
#24252=CARTESIAN_POINT('Ctrl Pts',(18.8396250155427,0.343942123623612,4.35158077372017));
#24253=CARTESIAN_POINT('Ctrl Pts',(18.8873408516054,-0.109704578635382,
4.47944773466767));
#24254=CARTESIAN_POINT('Ctrl Pts',(18.9350566876684,-0.462607878309702,
4.16703046362027));
#24255=CARTESIAN_POINT('Ctrl Pts',(18.9827725237311,-0.39069124519864,3.70122654773242));
#24256=CARTESIAN_POINT('Ctrl Pts',(19.030488359794,0.0400031699426168,3.50979089028978));
#24257=CARTESIAN_POINT('Ctrl Pts',(19.0782041958568,0.433962058584907,3.76852180111673));
#24258=CARTESIAN_POINT('Ctrl Pts',(19.1259200319197,0.429406911488226,4.23982270375453));
#24259=CARTESIAN_POINT('Ctrl Pts',(19.1736358679825,0.0305207902517796,
4.49089072733801));
#24260=CARTESIAN_POINT('Ctrl Pts',(19.2213517040454,-0.396393042209671,
4.29116624277653));
#24261=CARTESIAN_POINT('Ctrl Pts',(19.2690675401082,-0.459293044881286,
3.82405931712685));
#24262=CARTESIAN_POINT('Ctrl Pts',(19.316783376171,-0.100417177000157,3.51852142809106));
#24263=CARTESIAN_POINT('Ctrl Pts',(19.3644992122339,0.350673329058588,3.65513271950473));
#24264=CARTESIAN_POINT('Ctrl Pts',(19.4122150482967,0.479735122332443,4.10844094226069));
#24265=CARTESIAN_POINT('Ctrl Pts',(19.4599308843596,0.168248769032157,4.46216617689766));
#24266=CARTESIAN_POINT('Ctrl Pts',(19.5076467204224,-0.297743013815871,
4.39147710422109));
#24267=CARTESIAN_POINT('Ctrl Pts',(19.5553625564852,-0.490312813065352,
3.96128857502183));
#24268=CARTESIAN_POINT('Ctrl Pts',(19.603078392548,-0.232620797759261,3.56664935826393));
#24269=CARTESIAN_POINT('Ctrl Pts',(19.6507942286109,0.238690449241969,3.56996267500769));
#24270=CARTESIAN_POINT('Ctrl Pts',(19.6985100646737,0.490808633485035,3.96818593857384));
#24271=CARTESIAN_POINT('Ctrl Pts',(19.7462259007366,0.292209604061002,4.39562444172689));
#24272=CARTESIAN_POINT('Ctrl Pts',(19.7939417367994,-0.174729824492781,
4.45975512619968));
#24273=CARTESIAN_POINT('Ctrl Pts',(19.8416575728622,-0.481212499922896,
4.10168523844358));
#24274=CARTESIAN_POINT('Ctrl Pts',(19.8893734089251,-0.345789702982467,
3.65023692191923));
#24275=CARTESIAN_POINT('Ctrl Pts',(19.9370892449879,0.107175910646637,3.51998011832295));
#24276=CARTESIAN_POINT('Ctrl Pts',(19.9848050810508,0.461722480014006,3.83053541934297));
#24277=CARTESIAN_POINT('Ctrl Pts',(20.0325209171136,0.392257955100357,4.29670800504879));
#24278=CARTESIAN_POINT('Ctrl Pts',(20.0802367531764,-0.0374150865130887,
4.49041783929577));
#24279=CARTESIAN_POINT('Ctrl Pts',(20.1279525892393,-0.432744382500041,
4.23375285658289));
#24280=CARTESIAN_POINT('Ctrl Pts',(20.1756684253021,-0.430649333670284,
3.76246031529274));
#24281=CARTESIAN_POINT('Ctrl Pts',(20.223384261365,-0.033136228617316,3.50924504180455));
#24282=CARTESIAN_POINT('Ctrl Pts',(20.2711000974278,0.394908089060633,3.70680919012016));
#24283=CARTESIAN_POINT('Ctrl Pts',(20.3188159334906,0.460110046434968,4.17340395051402));
#24284=CARTESIAN_POINT('Ctrl Pts',(20.3665317695535,0.103149962306437,4.48116018402389));
#24285=CARTESIAN_POINT('Ctrl Pts',(20.4142476056163,-0.34923165553999,4.34628168153608));
#24286=CARTESIAN_POINT('Ctrl Pts',(20.4540108023354,-0.457800032585507,
3.97025345815189));
#24287=CARTESIAN_POINT('Ctrl Pts',(20.4858213597105,-0.325993724402262,
3.71529210935379));
#24288=CARTESIAN_POINT('Ctrl Pts',(20.509679277742,-0.15096738523986,3.59329490328468));
#24289=CARTESIAN_POINT('Ctrl Pts',(20.5335371957734,0.0630371972956549,
3.57102347342756));
#24290=CARTESIAN_POINT('Ctrl Pts',(20.5573951138048,0.260511246441404,3.65349437971329));
#24291=CARTESIAN_POINT('Ctrl Pts',(20.5812530318362,0.394877283734959,3.82077798440408));
#24292=CARTESIAN_POINT('Ctrl Pts',(20.6051109498677,0.432370081305563,4.03184236506754));
#24293=CARTESIAN_POINT('Ctrl Pts',(20.6289688678991,0.364303478986858,4.23514367899931));
#24294=CARTESIAN_POINT('Ctrl Pts',(20.6528267859305,0.207066376217976,4.38093363836299));
#24295=CARTESIAN_POINT('Ctrl Pts',(20.6766847039619,-0.000757290757721993,
4.43358147160167));
#24296=CARTESIAN_POINT('Ctrl Pts',(20.7005426219933,-0.208420567790133,
4.38020336888205));
#24297=CARTESIAN_POINT('Ctrl Pts',(20.7244005400248,-0.365106210756856,
4.23385701605743));
#24298=CARTESIAN_POINT('Ctrl Pts',(20.7482584580562,-0.432520392530856,
4.03032528343114));
#24299=CARTESIAN_POINT('Ctrl Pts',(20.7721163760876,-0.394167874571092,
3.81937870627435));
#24300=CARTESIAN_POINT('Ctrl Pts',(20.795974294119,-0.259432524437891,3.65259868360638));
#24301=CARTESIAN_POINT('Ctrl Pts',(20.8198322121504,-0.0612578225112809,
3.57076788979259));
#24302=CARTESIAN_POINT('Ctrl Pts',(20.8436901301819,0.151895538690754,3.5938959627232));
#24303=CARTESIAN_POINT('Ctrl Pts',(20.8675480482132,0.327906592802717,3.71632757520176));
#24304=CARTESIAN_POINT('Ctrl Pts',(20.8914059662447,0.423735399567132,3.90812480123879));
#24305=CARTESIAN_POINT('Ctrl Pts',(20.9152638842761,0.415949440063929,4.12238802732943));
#24306=CARTESIAN_POINT('Ctrl Pts',(20.9391218023075,0.30645246920106,4.30672404095661));
#24307=CARTESIAN_POINT('Ctrl Pts',(20.962979720339,0.122019544809087,4.41605767475162));
#24308=CARTESIAN_POINT('Ctrl Pts',(20.9868376383703,-0.0922504941031022,
4.42365387220386));
#24309=CARTESIAN_POINT('Ctrl Pts',(21.0106955564018,-0.28396276796243,4.32765515869354));
#24310=CARTESIAN_POINT('Ctrl Pts',(21.0345534744332,-0.40623841344949,4.15153583326342));
#24311=CARTESIAN_POINT('Ctrl Pts',(21.0584113924646,-0.429177699343215,
3.93836186909709));
#24312=CARTESIAN_POINT('Ctrl Pts',(21.082269310496,-0.347171348131155,3.74026010679315));
#24313=CARTESIAN_POINT('Ctrl Pts',(21.1061272285274,-0.180272145040548,
3.605671823621));
#24314=CARTESIAN_POINT('Ctrl Pts',(21.1299851465589,0.0307085077608185,
3.56750752082027));
#24315=CARTESIAN_POINT('Ctrl Pts',(21.1538430645903,0.234180094072738,3.63509941005724));
#24316=CARTESIAN_POINT('Ctrl Pts',(21.1777009826217,0.380388268371489,3.79191943321731));
#24317=CARTESIAN_POINT('Ctrl Pts',(21.2015589006531,0.433581149524578,3.99962082296209));
#24318=CARTESIAN_POINT('Ctrl Pts',(21.2254168186846,0.380751629084578,4.2074149318183));
#24319=CARTESIAN_POINT('Ctrl Pts',(21.2492747367159,0.234817963878357,4.36449043997717));
#24320=CARTESIAN_POINT('Ctrl Pts',(21.2731326547474,0.0314649101850846,
4.43243810704058));
#24321=CARTESIAN_POINT('Ctrl Pts',(21.2969905727788,-0.179582171132277,
4.39464287755545));
#24322=CARTESIAN_POINT('Ctrl Pts',(21.3208484908102,-0.346716519889314,
4.26034671465164));
#24323=CARTESIAN_POINT('Ctrl Pts',(21.3447064088417,-0.429069235164158,
4.0623886883135));
#24324=CARTESIAN_POINT('Ctrl Pts',(21.368564326873,-0.406502834830527,3.8491749282489));
#24325=CARTESIAN_POINT('Ctrl Pts',(21.3924222449045,-0.284535418465691,
3.67284200661995));
#24326=CARTESIAN_POINT('Ctrl Pts',(21.4162801629359,-0.0929913416969399,
3.5765081259772));
#24327=CARTESIAN_POINT('Ctrl Pts',(21.4401380809674,0.121291651150069,3.58372954422009));
#24328=CARTESIAN_POINT('Ctrl Pts',(21.4639959989987,0.305915531372611,3.69274042788069));
#24329=CARTESIAN_POINT('Ctrl Pts',(21.4878539170302,0.415734731202803,3.87688464650718));
#24330=CARTESIAN_POINT('Ctrl Pts',(21.5117118350615,0.423895464867194,4.09113392265755));
#24331=CARTESIAN_POINT('Ctrl Pts',(21.535569753093,0.328402210690932,4.28309847227994));
#24332=CARTESIAN_POINT('Ctrl Pts',(21.5594276711244,0.152605670504114,4.40583773398234));
#24333=CARTESIAN_POINT('Ctrl Pts',(21.5832855891559,-0.0605071130159612,
4.42933861492812));
#24334=CARTESIAN_POINT('Ctrl Pts',(21.6071435071872,-0.258824259222961,
4.34785450957493));
#24335=CARTESIAN_POINT('Ctrl Pts',(21.6310014252187,-0.39385182381868,4.18131050126406));
#24336=CARTESIAN_POINT('Ctrl Pts',(21.6548593432501,-0.432571889182456,
3.97043113659525));
#24337=CARTESIAN_POINT('Ctrl Pts',(21.6787172612815,-0.365516344619441,
3.76678216446856));
#24338=CARTESIAN_POINT('Ctrl Pts',(21.702575179313,-0.209082097331647,3.62016130585559));
#24339=CARTESIAN_POINT('Ctrl Pts',(21.7264330973443,-0.00152158196427748,
3.56642135455923));
#24340=CARTESIAN_POINT('Ctrl Pts',(21.7502910153758,0.206411001640417,3.61870319251831));
#24341=CARTESIAN_POINT('Ctrl Pts',(21.7741489334072,0.363870472821225,3.76422248622317));
#24342=CARTESIAN_POINT('Ctrl Pts',(21.7980068514386,0.432353701764573,3.96739580449697));
#24343=CARTESIAN_POINT('Ctrl Pts',(21.82186476947,0.395114673548107,4.17854173669174));
#24344=CARTESIAN_POINT('Ctrl Pts',(21.8457226875014,0.261259344941517,4.3460293508861));
#24345=CARTESIAN_POINT('Ctrl Pts',(21.8695806055329,0.0635189899350569,
4.42890336313855));
#24346=CARTESIAN_POINT('Ctrl Pts',(21.8934385235643,-0.14975348833307,4.40689882001058));
#24347=CARTESIAN_POINT('Ctrl Pts',(21.9172964415957,-0.326407159500644,
4.28539643168872));
#24348=CARTESIAN_POINT('Ctrl Pts',(21.9411543596271,-0.423245389017799,
4.09410684177624));
#24349=CARTESIAN_POINT('Ctrl Pts',(21.9650122776585,-0.416588591947193,
3.87980556563057));
#24350=CARTESIAN_POINT('Ctrl Pts',(21.98887019569,-0.30806453650007,3.69489510271888));
#24351=CARTESIAN_POINT('Ctrl Pts',(22.0127281137213,-0.12421031036921,3.58459109808296));
#24352=CARTESIAN_POINT('Ctrl Pts',(22.0365860317528,0.0900167200678817,
3.57586588547707));
#24353=CARTESIAN_POINT('Ctrl Pts',(22.0604439497842,0.282232210442068,3.67085301705332));
#24354=CARTESIAN_POINT('Ctrl Pts',(22.0843018678157,0.405434237512275,3.8463255517439));
#24355=CARTESIAN_POINT('Ctrl Pts',(22.108159785847,0.429496549703537,4.05937567504088));
#24356=CARTESIAN_POINT('Ctrl Pts',(22.1320177038785,0.348535256241736,4.25790682842971));
#24357=CARTESIAN_POINT('Ctrl Pts',(22.1558756219099,0.182347598717988,4.39337273702606));
#24358=CARTESIAN_POINT('Ctrl Pts',(22.1797335399413,-0.0284290137391457,
4.43264829616218));
#24359=CARTESIAN_POINT('Ctrl Pts',(22.2035914579727,-0.232253957950086,
4.36612956178204));
#24360=CARTESIAN_POINT('Ctrl Pts',(22.2274493760041,-0.379286482964224,
4.21008217638027));
#24361=CARTESIAN_POINT('Ctrl Pts',(22.2513072940356,-0.433573131350875,
4.00266397632408));
#24362=CARTESIAN_POINT('Ctrl Pts',(22.275165212067,-0.381839338801546,3.79459436150246));
#24363=CARTESIAN_POINT('Ctrl Pts',(22.2990231300984,-0.236735426869051,
3.63675202040985));
#24364=CARTESIAN_POINT('Ctrl Pts',(22.3228810481298,-0.0337432544318164,
3.56773370504276));
#24365=CARTESIAN_POINT('Ctrl Pts',(22.3467389661613,0.177500062688638,3.60441627341574));
#24366=CARTESIAN_POINT('Ctrl Pts',(22.3705968841926,0.345339779804043,3.73782983856348));
#24367=CARTESIAN_POINT('Ctrl Pts',(22.3944548022241,0.428734513273282,3.93535114928888));
#24368=CARTESIAN_POINT('Ctrl Pts',(22.4183127202555,0.407291980919218,4.1486808655136));
#24369=CARTESIAN_POINT('Ctrl Pts',(22.4421706382869,0.286255462618544,4.32565405918856));
#24370=CARTESIAN_POINT('Ctrl Pts',(22.4660285563183,0.0952216904214238,
4.42299596654013));
#24371=CARTESIAN_POINT('Ctrl Pts',(22.4898864743497,-0.119096386717928,
4.41690383452019));
#24372=CARTESIAN_POINT('Ctrl Pts',(22.5137443923812,-0.304292138366774,
4.30886736509782));
#24373=CARTESIAN_POINT('Ctrl Pts',(22.5376023104126,-0.415080201412036,
4.12530439950267));
#24374=CARTESIAN_POINT('Ctrl Pts',(22.561460228444,-0.424369795825249,3.91110111771763));
#24375=CARTESIAN_POINT('Ctrl Pts',(22.5853181464754,-0.329889515310188,
3.71863599132299));
#24376=CARTESIAN_POINT('Ctrl Pts',(22.6091760645068,-0.154742073939436,
3.59497211022641));
#24377=CARTESIAN_POINT('Ctrl Pts',(22.6330339825383,0.0582436639512456,
3.57034842802071));
#24378=CARTESIAN_POINT('Ctrl Pts',(22.6568919005697,0.256987911016647,3.65078654733876));
#24379=CARTESIAN_POINT('Ctrl Pts',(22.6807498186011,0.39289034562191,3.81661632308649));
#24380=CARTESIAN_POINT('Ctrl Pts',(22.7046077366325,0.432722782933869,4.02728943245291));
#24381=CARTESIAN_POINT('Ctrl Pts',(22.7284656546639,0.366738191089385,4.2312875884069));
#24382=CARTESIAN_POINT('Ctrl Pts',(22.7523235726953,0.211084664509997,4.37873330099785));
#24383=CARTESIAN_POINT('Ctrl Pts',(22.7761814907268,0.00379901600965994,
4.43356145647204));
#24384=CARTESIAN_POINT('Ctrl Pts',(22.8000394087582,-0.204384723485633,
4.3823852668741));
#24385=CARTESIAN_POINT('Ctrl Pts',(22.8238973267896,-0.36265185203719,4.2376794731));
#24386=CARTESIAN_POINT('Ctrl Pts',(22.8398026054772,-0.408954280604672,
4.10250106973657));
#24387=CARTESIAN_POINT('Ctrl Pts',(22.847755244821,-0.414526965927561,4.03345758723954));
#24388=CARTESIAN_POINT('',(22.8,-0.592174260192535,4.04779597854866));
#24389=CARTESIAN_POINT('Ctrl Pts',(22.8,-0.19576256658266,4.36695865185836));
#24390=CARTESIAN_POINT('Ctrl Pts',(22.8,-0.195886593570853,4.36694806728808));
#24391=CARTESIAN_POINT('Ctrl Pts',(22.8,-0.196010613870461,4.36693742279878));
#24392=CARTESIAN_POINT('Ctrl Pts',(22.8,-0.196134627427637,4.36692671841166));
#24393=CARTESIAN_POINT('Ctrl Pts',(22.8,-0.216622178843513,4.36515830948628));
#24394=CARTESIAN_POINT('Ctrl Pts',(22.8,-0.236921239981942,4.36175743074964));
#24395=CARTESIAN_POINT('Ctrl Pts',(22.8,-0.256857422940798,4.35688458679081));
#24396=CARTESIAN_POINT('Ctrl Pts',(22.8,-0.271809560159941,4.35322995382169));
#24397=CARTESIAN_POINT('Ctrl Pts',(22.8,-0.286558947067823,4.34874691155445));
#24398=CARTESIAN_POINT('Ctrl Pts',(22.8,-0.301048271828705,4.34349077646485));
#24399=CARTESIAN_POINT('Ctrl Pts',(22.8,-0.310003423377303,4.3402422133286));
#24400=CARTESIAN_POINT('Ctrl Pts',(22.8,-0.318859482942331,4.33669811041118));
#24401=CARTESIAN_POINT('Ctrl Pts',(22.8,-0.327604744452034,4.33286912874946));
#24402=CARTESIAN_POINT('Ctrl Pts',(22.8,-0.333457186121174,4.33030672489195));
#24403=CARTESIAN_POINT('Ctrl Pts',(22.8,-0.33926207870774,4.32761569029118));
#24404=CARTESIAN_POINT('Ctrl Pts',(22.8,-0.345009487597299,4.32480202294401));
#24405=CARTESIAN_POINT('Ctrl Pts',(22.8,-0.365309066997251,4.31486428146495));
#24406=CARTESIAN_POINT('Ctrl Pts',(22.8,-0.384828901796994,4.30343044333042));
#24407=CARTESIAN_POINT('Ctrl Pts',(22.8,-0.403416958856431,4.29067119823496));
#24408=CARTESIAN_POINT('Ctrl Pts',(22.8,-0.409874425773003,4.28623865303559));
#24409=CARTESIAN_POINT('Ctrl Pts',(22.8,-0.416219739836017,4.28164578247975));
#24410=CARTESIAN_POINT('Ctrl Pts',(22.8,-0.422447327171508,4.27689854297234));
#24411=CARTESIAN_POINT('Ctrl Pts',(22.8,-0.43500295340691,4.2673274905416));
#24412=CARTESIAN_POINT('Ctrl Pts',(22.8,-0.447079966647781,4.25712966465555));
#24413=CARTESIAN_POINT('Ctrl Pts',(22.8,-0.458660056443695,4.24636133358853));
#24414=CARTESIAN_POINT('Ctrl Pts',(22.8,-0.465333929961841,4.24015529539631));
#24415=CARTESIAN_POINT('Ctrl Pts',(22.8,-0.471842796551704,4.23375955955572));
#24416=CARTESIAN_POINT('Ctrl Pts',(22.8,-0.478183280583292,4.22718326898633));
#24417=CARTESIAN_POINT('Ctrl Pts',(22.8,-0.48330469601013,4.22187138494));
#24418=CARTESIAN_POINT('Ctrl Pts',(22.8,-0.488310096860405,4.21644792156372));
#24419=CARTESIAN_POINT('Ctrl Pts',(22.8,-0.49319389770791,4.21092357737429));
#24420=CARTESIAN_POINT('Ctrl Pts',(22.8,-0.509882204568999,4.19204648678071));
#24421=CARTESIAN_POINT('Ctrl Pts',(22.8,-0.525164669297395,4.17198027236651));
#24422=CARTESIAN_POINT('Ctrl Pts',(22.8,-0.538985569877159,4.15095378743758));
#24423=CARTESIAN_POINT('Ctrl Pts',(22.8,-0.553292287721507,4.12918820238033));
#24424=CARTESIAN_POINT('Ctrl Pts',(22.8,-0.566034197593199,4.10639346234103));
#24425=CARTESIAN_POINT('Ctrl Pts',(22.8,-0.577149101532509,4.08276767497818));
#24426=CARTESIAN_POINT('Ctrl Pts',(22.8,-0.582543745751794,4.07130084468266));
#24427=CARTESIAN_POINT('Ctrl Pts',(22.8,-0.587554988912119,4.05963744408228));
#24428=CARTESIAN_POINT('Ctrl Pts',(22.8,-0.592174260192535,4.04779597854866));
#24429=CARTESIAN_POINT('Ctrl Pts',(4.,0.254721014554616,3.46322028700966));
#24430=CARTESIAN_POINT('Ctrl Pts',(4.,0.254552373521139,3.46319452321125));
#24431=CARTESIAN_POINT('Ctrl Pts',(4.,0.254383724765285,3.46316883668624));
#24432=CARTESIAN_POINT('Ctrl Pts',(4.,0.254215068323085,3.46314322746093));
#24433=CARTESIAN_POINT('Ctrl Pts',(4.,0.228435861761457,3.4592288468388));
#24434=CARTESIAN_POINT('Ctrl Pts',(4.,0.202474691352968,3.45711700011808));
#24435=CARTESIAN_POINT('Ctrl Pts',(4.,0.176517231963435,3.45683380906617));
#24436=CARTESIAN_POINT('Ctrl Pts',(4.,0.151199179447316,3.45655759382427));
#24437=CARTESIAN_POINT('Ctrl Pts',(4.,0.125883695414598,3.45802192769867));
#24438=CARTESIAN_POINT('Ctrl Pts',(4.,0.1007794950383,3.46128259448669));
#24439=CARTESIAN_POINT('Ctrl Pts',(4.,0.0854593772715275,3.46327245269535));
#24440=CARTESIAN_POINT('Ctrl Pts',(4.,0.0702187270328167,3.46593187194604));
#24441=CARTESIAN_POINT('Ctrl Pts',(4.,0.0551140352340102,3.4692772918897));
#24442=CARTESIAN_POINT('Ctrl Pts',(4.,0.0468842919617017,3.47110003330284));
#24443=CARTESIAN_POINT('Ctrl Pts',(4.,0.0386923719445779,3.47312744960567));
#24444=CARTESIAN_POINT('Ctrl Pts',(4.,0.0305707631998946,3.47535548770785));
#24445=CARTESIAN_POINT('Ctrl Pts',(4.,0.0102648423897012,3.48092610391051));
#24446=CARTESIAN_POINT('Ctrl Pts',(4.,-0.00963556638195036,3.48775588581666));
#24447=CARTESIAN_POINT('Ctrl Pts',(4.,-0.0289965775380143,3.49587186612014));
#24448=CARTESIAN_POINT('Ctrl Pts',(4.,-0.047965755796229,3.50382359322137));
#24449=CARTESIAN_POINT('Ctrl Pts',(4.,-0.0664174073931304,3.51301096346156));
#24450=CARTESIAN_POINT('Ctrl Pts',(4.,-0.0841982143338667,3.52340033683134));
#24451=CARTESIAN_POINT('Ctrl Pts',(4.,-0.0930898199841631,3.5285957259532));
#24452=CARTESIAN_POINT('Ctrl Pts',(4.,-0.101813128894432,3.53409169793663));
#24453=CARTESIAN_POINT('Ctrl Pts',(4.,-0.110345561972859,3.53988353361915));
#24454=CARTESIAN_POINT('Ctrl Pts',(4.,-0.11586100642067,3.5436274303089));
#24455=CARTESIAN_POINT('Ctrl Pts',(4.,-0.121288652521606,3.54748953413154));
#24456=CARTESIAN_POINT('Ctrl Pts',(4.,-0.126621987542688,3.55146681430013));
#24457=CARTESIAN_POINT('Ctrl Pts',(4.,-0.143297831161627,3.56390265451229));
#24458=CARTESIAN_POINT('Ctrl Pts',(4.,-0.159061930875806,3.57746928852925));
#24459=CARTESIAN_POINT('Ctrl Pts',(4.,-0.173743808224101,3.59211536896244));
#24460=CARTESIAN_POINT('Ctrl Pts',(4.,-0.187864697165731,3.60620182877415));
#24461=CARTESIAN_POINT('Ctrl Pts',(4.,-0.200984288190684,3.62128798311348));
#24462=CARTESIAN_POINT('Ctrl Pts',(4.,-0.212904831975564,3.63731335989365));
#24463=CARTESIAN_POINT('Ctrl Pts',(4.,-0.21528245268753,3.64050971304978));
#24464=CARTESIAN_POINT('Ctrl Pts',(4.,-0.217612227418936,3.64374335030505));
#24465=CARTESIAN_POINT('Ctrl Pts',(4.,-0.219892372743211,3.64701365460636));
#24466=CARTESIAN_POINT('Ctrl Pts',(22.8,-0.592174260192532,4.04779597854869));
#24467=CARTESIAN_POINT('Ctrl Pts',(22.7920473606562,-0.584213376873468,
4.14642833911734));
#24468=CARTESIAN_POINT('Ctrl Pts',(22.7840947213124,-0.551140611244481,
4.24298318064208));
#24469=CARTESIAN_POINT('Ctrl Pts',(22.7761420819686,-0.496922031827459,
4.32571394759471));
#24470=CARTESIAN_POINT('Ctrl Pts',(22.7681894426248,-0.442703452410443,
4.40844471454734));
#24471=CARTESIAN_POINT('Ctrl Pts',(22.760236803281,-0.367339059205388,4.47735140692785));
#24472=CARTESIAN_POINT('Ctrl Pts',(22.7522841639372,-0.280089901523161,
4.52398941366922));
#24473=CARTESIAN_POINT('Ctrl Pts',(22.7444712463773,-0.194373644734646,
4.56980802634291));
#24474=CARTESIAN_POINT('Ctrl Pts',(22.7366583288174,-0.0971865673270821,
4.59413356703531));
#24475=CARTESIAN_POINT('Ctrl Pts',(22.7288454112575,-7.11440487624268E-7,
4.59414971000239));
#24476=CARTESIAN_POINT('Origin',(27.2,0.3,2.9));
#24477=CARTESIAN_POINT('',(29.2,0.3,3.04606079858305));
#24478=CARTESIAN_POINT('',(27.2,0.3,3.04606079858305));
#24479=CARTESIAN_POINT('',(23.3,0.3,3.04606079858305));
#24480=CARTESIAN_POINT('',(29.2,0.3,3.35));
#24481=CARTESIAN_POINT('',(29.2,0.3,2.9));
#24482=CARTESIAN_POINT('',(27.2,0.3,3.35));
#24483=CARTESIAN_POINT('',(27.2,0.3,3.35));
#24484=CARTESIAN_POINT('',(27.2,0.3,2.9));
#24485=CARTESIAN_POINT('Origin',(27.2,0.,3.125));
#24486=CARTESIAN_POINT('',(27.2,-0.3,3.04606079858305));
#24487=CARTESIAN_POINT('Origin',(27.2,0.,4.));
#24488=CARTESIAN_POINT('',(27.2,-0.3,3.35));
#24489=CARTESIAN_POINT('',(27.2,0.3,3.35));
#24490=CARTESIAN_POINT('',(27.2,-0.3,3.35));
#24491=CARTESIAN_POINT('Origin',(27.2,0.3,3.35));
#24492=CARTESIAN_POINT('',(29.2,-0.3,3.35));
#24493=CARTESIAN_POINT('',(29.2,0.3,3.35));
#24494=CARTESIAN_POINT('',(27.2,-0.3,3.35));
#24495=CARTESIAN_POINT('Origin',(27.2,-0.3,3.35));
#24496=CARTESIAN_POINT('',(29.2,-0.3,3.04606079858305));
#24497=CARTESIAN_POINT('',(23.3,-0.3,3.04606079858305));
#24498=CARTESIAN_POINT('',(29.2,-0.3,3.35));
#24499=CARTESIAN_POINT('Origin',(29.2,0.,3.125));
#24500=CARTESIAN_POINT('Origin',(29.2,0.,4.));
#24501=CARTESIAN_POINT('Origin',(23.3,0.,4.));
#24502=CARTESIAN_POINT('',(29.4,-1.22464679914735E-16,5.));
#24503=CARTESIAN_POINT('Origin',(29.4,0.,4.));
#24504=CARTESIAN_POINT('',(23.3,-1.22464679914735E-16,5.));
#24505=CARTESIAN_POINT('',(23.3,-1.22464679914735E-16,5.));
#24506=CARTESIAN_POINT('Origin',(23.3,0.,4.));
#24507=CARTESIAN_POINT('Origin',(29.4,0.,4.));
#24508=CARTESIAN_POINT('Origin',(22.8,0.,4.));
#24509=CARTESIAN_POINT('',(22.8,-1.65327317884893E-16,5.35));
#24510=CARTESIAN_POINT('Origin',(22.8,0.,4.));
#24511=CARTESIAN_POINT('Origin',(22.8,0.,4.));
#24512=CARTESIAN_POINT('Origin',(22.8,0.,4.));
#24513=CARTESIAN_POINT('',(23.3,-1.65327317884893E-16,5.35));
#24514=CARTESIAN_POINT('Origin',(23.3,0.,4.));
#24515=CARTESIAN_POINT('',(22.8,-1.65327317884893E-16,5.35));
#24516=CARTESIAN_POINT('Origin',(23.3,0.,4.));
#24517=CARTESIAN_POINT('Origin',(4.,0.,4.));
#24518=CARTESIAN_POINT('Origin',(4.,0.,4.));
#24519=CARTESIAN_POINT('',(0.,0.,0.));
#24520=CARTESIAN_POINT('Origin',(24.7,0.,4.));
#24521=CARTESIAN_POINT('',(25.4,-1.23689326713883E-16,5.01));
#24522=CARTESIAN_POINT('Origin',(25.4,0.,4.));
#24523=CARTESIAN_POINT('',(24.7,-1.23689326713883E-16,5.01));
#24524=CARTESIAN_POINT('',(24.7,-1.23689326713883E-16,5.01));
#24525=CARTESIAN_POINT('Origin',(24.7,0.,4.));
#24526=CARTESIAN_POINT('Origin',(24.7,0.,4.));
#24527=CARTESIAN_POINT('',(25.4,-1.65327317884893E-16,5.35));
#24528=CARTESIAN_POINT('Origin',(25.4,0.,4.));
#24529=CARTESIAN_POINT('',(24.7,-1.65327317884893E-16,5.35));
#24530=CARTESIAN_POINT('',(24.7,-1.65327317884893E-16,5.35));
#24531=CARTESIAN_POINT('Origin',(24.7,0.,4.));
#24532=CARTESIAN_POINT('Origin',(25.4,0.,4.));
#24533=CARTESIAN_POINT('Origin',(24.7,0.,4.));
#24534=CARTESIAN_POINT('',(0.,0.,0.));
#24535=CARTESIAN_POINT('Origin',(25.8,0.99,4.));
#24536=CARTESIAN_POINT('',(25.6809411910021,0.99,4.17298843892006));
#24537=CARTESIAN_POINT('',(25.9190588089979,0.99,4.17298843892006));
#24538=CARTESIAN_POINT('',(25.4,0.99,4.17298843892006));
#24539=CARTESIAN_POINT('Origin',(25.8,0.99,4.));
#24540=CARTESIAN_POINT('Origin',(25.8,0.99,4.));
#24541=CARTESIAN_POINT('',(25.6809411910021,0.99,3.82701156107994));
#24542=CARTESIAN_POINT('',(25.59,1.005,4.));
#24543=CARTESIAN_POINT('Ctrl Pts',(25.6809411910021,0.989999999999999,3.82701156107994));
#24544=CARTESIAN_POINT('Ctrl Pts',(25.6701985776047,0.99129192197638,3.83440513468868));
#24545=CARTESIAN_POINT('Ctrl Pts',(25.6603122906273,0.992653949439047,3.84270286127439));
#24546=CARTESIAN_POINT('Ctrl Pts',(25.6329072257467,0.996748084390898,3.87010792615492));
#24547=CARTESIAN_POINT('Ctrl Pts',(25.6167579436671,0.999695893276376,3.89366983224072));
#24548=CARTESIAN_POINT('Ctrl Pts',(25.5953022060351,1.00385029472357,3.94538709536759));
#24549=CARTESIAN_POINT('Ctrl Pts',(25.59,1.005,3.97354876917015));
#24550=CARTESIAN_POINT('Ctrl Pts',(25.59,1.005,4.));
#24551=CARTESIAN_POINT('',(25.9190588089979,0.99,3.82701156107994));
#24552=CARTESIAN_POINT('Origin',(25.8,0.99,4.));
#24553=CARTESIAN_POINT('Ctrl Pts',(25.9190588089979,0.99,4.17298843892006));
#24554=CARTESIAN_POINT('Ctrl Pts',(25.9298014223953,0.991291921976381,4.16559486531132));
#24555=CARTESIAN_POINT('Ctrl Pts',(25.9396877093727,0.992653949439047,4.15729713872561));
#24556=CARTESIAN_POINT('Ctrl Pts',(25.9670927742533,0.996748084390898,4.12989207384508));
#24557=CARTESIAN_POINT('Ctrl Pts',(25.9832420563329,0.999695893276376,4.10633016775929));
#24558=CARTESIAN_POINT('Ctrl Pts',(26.0046977939649,1.00385029472357,4.05461290463241));
#24559=CARTESIAN_POINT('Ctrl Pts',(26.01,1.005,4.02645123082985));
#24560=CARTESIAN_POINT('Ctrl Pts',(26.01,1.005,3.97354876917015));
#24561=CARTESIAN_POINT('Ctrl Pts',(26.0046977939649,1.00385029472357,3.94538709536759));
#24562=CARTESIAN_POINT('Ctrl Pts',(25.9832420563329,0.999695893276376,3.89366983224072));
#24563=CARTESIAN_POINT('Ctrl Pts',(25.9670927742533,0.996748084390898,3.87010792615492));
#24564=CARTESIAN_POINT('Ctrl Pts',(25.9396877093727,0.992653949439047,3.84270286127439));
#24565=CARTESIAN_POINT('Ctrl Pts',(25.9298014223953,0.991291921976381,3.83440513468868));
#24566=CARTESIAN_POINT('Ctrl Pts',(25.9190588089979,0.99,3.82701156107994));
#24567=CARTESIAN_POINT('Ctrl Pts',(25.59,1.005,4.));
#24568=CARTESIAN_POINT('Ctrl Pts',(25.59,1.005,4.02645123082985));
#24569=CARTESIAN_POINT('Ctrl Pts',(25.5953022060351,1.00385029472357,4.05461290463241));
#24570=CARTESIAN_POINT('Ctrl Pts',(25.6167579436671,0.999695893276376,4.10633016775929));
#24571=CARTESIAN_POINT('Ctrl Pts',(25.6329072257467,0.996748084390898,4.12989207384508));
#24572=CARTESIAN_POINT('Ctrl Pts',(25.6603122906273,0.992653949439047,4.15729713872561));
#24573=CARTESIAN_POINT('Ctrl Pts',(25.6701985776047,0.991291921976381,4.16559486531132));
#24574=CARTESIAN_POINT('Ctrl Pts',(25.6809411910021,0.99,4.17298843892006));
#24575=CARTESIAN_POINT('',(25.59,1.5,4.));
#24576=CARTESIAN_POINT('',(25.59,0.99,4.));
#24577=CARTESIAN_POINT('',(25.8,1.48522725533839,4.21));
#24578=CARTESIAN_POINT('Ctrl Pts',(25.8,1.48522725533839,4.21));
#24579=CARTESIAN_POINT('Ctrl Pts',(25.7735944730755,1.48522725533839,4.21));
#24580=CARTESIAN_POINT('Ctrl Pts',(25.7454529259093,1.48600415954412,4.2047157372696));
#24581=CARTESIAN_POINT('Ctrl Pts',(25.6937237310949,1.48880073282317,4.18327376303633));
#24582=CARTESIAN_POINT('Ctrl Pts',(25.670133075872,1.49077897157582,4.16711792397039));
#24583=CARTESIAN_POINT('Ctrl Pts',(25.632882321789,1.49448481141327,4.12986716988737));
#24584=CARTESIAN_POINT('Ctrl Pts',(25.6167262899986,1.49645455657129,4.10627640830577));
#24585=CARTESIAN_POINT('Ctrl Pts',(25.5952841751738,1.49923165515646,4.0545468514059));
#24586=CARTESIAN_POINT('Ctrl Pts',(25.59,1.5,4.02640517850928));
#24587=CARTESIAN_POINT('Ctrl Pts',(25.59,1.5,4.));
#24588=CARTESIAN_POINT('Ctrl Pts',(25.59,1.5,4.));
#24589=CARTESIAN_POINT('Ctrl Pts',(25.59,1.5,3.97359482149072));
#24590=CARTESIAN_POINT('Ctrl Pts',(25.5952841751738,1.49923165515646,3.9454531485941));
#24591=CARTESIAN_POINT('Ctrl Pts',(25.6167262899986,1.49645455657129,3.89372359169423));
#24592=CARTESIAN_POINT('Ctrl Pts',(25.632882321789,1.49448481141327,3.87013283011263));
#24593=CARTESIAN_POINT('Ctrl Pts',(25.670133075872,1.49077897157582,3.83288207602961));
#24594=CARTESIAN_POINT('Ctrl Pts',(25.6937237310949,1.48880073282317,3.81672623696366));
#24595=CARTESIAN_POINT('Ctrl Pts',(25.7454529259093,1.48600415954412,3.7952842627304));
#24596=CARTESIAN_POINT('Ctrl Pts',(25.7735944730755,1.48522725533839,3.79));
#24597=CARTESIAN_POINT('Ctrl Pts',(25.8264055269245,1.48522725533839,3.79));
#24598=CARTESIAN_POINT('Ctrl Pts',(25.8545470740907,1.48600415954412,3.7952842627304));
#24599=CARTESIAN_POINT('Ctrl Pts',(25.9062762689051,1.48880073282317,3.81672623696367));
#24600=CARTESIAN_POINT('Ctrl Pts',(25.929866924128,1.49077897157582,3.83288207602961));
#24601=CARTESIAN_POINT('Ctrl Pts',(25.967117678211,1.49448481141327,3.87013283011263));
#24602=CARTESIAN_POINT('Ctrl Pts',(25.9832737100014,1.49645455657129,3.89372359169423));
#24603=CARTESIAN_POINT('Ctrl Pts',(26.0047158248262,1.49923165515646,3.9454531485941));
#24604=CARTESIAN_POINT('Ctrl Pts',(26.01,1.5,3.97359482149072));
#24605=CARTESIAN_POINT('Ctrl Pts',(26.01,1.5,4.02640517850928));
#24606=CARTESIAN_POINT('Ctrl Pts',(26.0047158248262,1.49923165515646,4.0545468514059));
#24607=CARTESIAN_POINT('Ctrl Pts',(25.9832737100014,1.49645455657129,4.10627640830577));
#24608=CARTESIAN_POINT('Ctrl Pts',(25.967117678211,1.49448481141327,4.12986716988737));
#24609=CARTESIAN_POINT('Ctrl Pts',(25.929866924128,1.49077897157582,4.16711792397039));
#24610=CARTESIAN_POINT('Ctrl Pts',(25.9062762689051,1.48880073282317,4.18327376303633));
#24611=CARTESIAN_POINT('Ctrl Pts',(25.8545470740907,1.48600415954412,4.20471573726959));
#24612=CARTESIAN_POINT('Ctrl Pts',(25.8264055269245,1.48522725533839,4.21));
#24613=CARTESIAN_POINT('Ctrl Pts',(25.8,1.48522725533839,4.21));
#24614=CARTESIAN_POINT('Origin',(25.8,0.99,4.));
#24615=CARTESIAN_POINT('',(25.4,0.99,3.82701156107994));
#24616=CARTESIAN_POINT('Origin',(25.4,0.,4.));
#24617=CARTESIAN_POINT('',(26.2,-1.23077003314309E-16,5.005));
#24618=CARTESIAN_POINT('Origin',(26.2,0.,4.));
#24619=CARTESIAN_POINT('',(25.4,-1.23077003314309E-16,5.005));
#24620=CARTESIAN_POINT('',(25.4,-1.23077003314309E-16,5.005));
#24621=CARTESIAN_POINT('Origin',(25.4,0.,4.));
#24622=CARTESIAN_POINT('Origin',(25.4,0.,4.));
#24623=CARTESIAN_POINT('',(26.2,-1.83697019872103E-16,5.5));
#24624=CARTESIAN_POINT('Origin',(26.2,0.,4.));
#24625=CARTESIAN_POINT('',(25.4,-1.83697019872103E-16,5.5));
#24626=CARTESIAN_POINT('',(25.4,-1.83697019872103E-16,5.5));
#24627=CARTESIAN_POINT('Origin',(25.4,0.,4.));
#24628=CARTESIAN_POINT('Origin',(26.2,0.,4.));
#24629=CARTESIAN_POINT('Origin',(25.4,0.,4.));
#24630=CARTESIAN_POINT('',(0.,0.,0.));
#24631=CARTESIAN_POINT('Origin',(28.7,0.,6.5));
#24632=CARTESIAN_POINT('',(28.8,-3.06161699786838E-17,6.75));
#24633=CARTESIAN_POINT('Origin',(28.8,0.,6.5));
#24634=CARTESIAN_POINT('',(29.4,3.06161699786838E-17,6.75));
#24635=CARTESIAN_POINT('',(28.7,-3.06161699786838E-17,6.75));
#24636=CARTESIAN_POINT('Origin',(29.4,0.,6.5));
#24637=CARTESIAN_POINT('Origin',(28.,0.99,4.));
#24638=CARTESIAN_POINT('',(27.844436508139,0.99,4.14106735979666));
#24639=CARTESIAN_POINT('',(28.155563491861,0.99,4.14106735979666));
#24640=CARTESIAN_POINT('',(27.,0.99,4.14106735979666));
#24641=CARTESIAN_POINT('Origin',(28.,0.99,4.));
#24642=CARTESIAN_POINT('Origin',(28.,0.99,4.));
#24643=CARTESIAN_POINT('',(27.844436508139,0.99,3.85893264020334));
#24644=CARTESIAN_POINT('',(27.79,1.,4.));
#24645=CARTESIAN_POINT('Ctrl Pts',(27.844436508139,0.99,3.85893264020334));
#24646=CARTESIAN_POINT('Ctrl Pts',(27.8287948476368,0.992457849824465,3.87618164330178));
#24647=CARTESIAN_POINT('Ctrl Pts',(27.815375956669,0.994938193049464,3.8970013568903));
#24648=CARTESIAN_POINT('Ctrl Pts',(27.7953025362756,0.998844492372413,3.94538588560165));
#24649=CARTESIAN_POINT('Ctrl Pts',(27.79,1.,3.97354792631755));
#24650=CARTESIAN_POINT('Ctrl Pts',(27.79,1.,4.));
#24651=CARTESIAN_POINT('',(28.155563491861,0.99,3.85893264020334));
#24652=CARTESIAN_POINT('Origin',(28.,0.99,4.));
#24653=CARTESIAN_POINT('Ctrl Pts',(28.155563491861,0.99,4.14106735979666));
#24654=CARTESIAN_POINT('Ctrl Pts',(28.1712051523632,0.992457849824465,4.12381835669823));
#24655=CARTESIAN_POINT('Ctrl Pts',(28.184624043331,0.994938193049464,4.1029986431097));
#24656=CARTESIAN_POINT('Ctrl Pts',(28.2046974637244,0.998844492372413,4.05461411439835));
#24657=CARTESIAN_POINT('Ctrl Pts',(28.21,1.,4.02645207368245));
#24658=CARTESIAN_POINT('Ctrl Pts',(28.21,1.,3.97354792631755));
#24659=CARTESIAN_POINT('Ctrl Pts',(28.2046974637244,0.998844492372413,3.94538588560165));
#24660=CARTESIAN_POINT('Ctrl Pts',(28.184624043331,0.994938193049464,3.8970013568903));
#24661=CARTESIAN_POINT('Ctrl Pts',(28.1712051523632,0.992457849824465,3.87618164330178));
#24662=CARTESIAN_POINT('Ctrl Pts',(28.155563491861,0.99,3.85893264020334));
#24663=CARTESIAN_POINT('Ctrl Pts',(27.79,1.,4.));
#24664=CARTESIAN_POINT('Ctrl Pts',(27.79,1.,4.02645207368245));
#24665=CARTESIAN_POINT('Ctrl Pts',(27.7953025362756,0.998844492372413,4.05461411439835));
#24666=CARTESIAN_POINT('Ctrl Pts',(27.815375956669,0.994938193049464,4.1029986431097));
#24667=CARTESIAN_POINT('Ctrl Pts',(27.8287948476368,0.992457849824465,4.12381835669823));
#24668=CARTESIAN_POINT('Ctrl Pts',(27.844436508139,0.99,4.14106735979666));
#24669=CARTESIAN_POINT('',(27.79,1.5,4.));
#24670=CARTESIAN_POINT('',(27.79,0.99,4.));
#24671=CARTESIAN_POINT('',(28.,1.48522725533839,4.21));
#24672=CARTESIAN_POINT('Ctrl Pts',(28.,1.48522725533839,4.21));
#24673=CARTESIAN_POINT('Ctrl Pts',(27.9735944730755,1.48522725533839,4.21));
#24674=CARTESIAN_POINT('Ctrl Pts',(27.9454529259093,1.48600415954412,4.20471573726959));
#24675=CARTESIAN_POINT('Ctrl Pts',(27.8937237310949,1.48880073282317,4.18327376303633));
#24676=CARTESIAN_POINT('Ctrl Pts',(27.870133075872,1.49077897157582,4.16711792397039));
#24677=CARTESIAN_POINT('Ctrl Pts',(27.832882321789,1.49448481141327,4.12986716988737));
#24678=CARTESIAN_POINT('Ctrl Pts',(27.8167262899986,1.49645455657129,4.10627640830576));
#24679=CARTESIAN_POINT('Ctrl Pts',(27.7952841751738,1.49923165515646,4.0545468514059));
#24680=CARTESIAN_POINT('Ctrl Pts',(27.79,1.5,4.02640517850928));
#24681=CARTESIAN_POINT('Ctrl Pts',(27.79,1.5,4.));
#24682=CARTESIAN_POINT('Ctrl Pts',(27.79,1.5,4.));
#24683=CARTESIAN_POINT('Ctrl Pts',(27.79,1.5,3.97359482149072));
#24684=CARTESIAN_POINT('Ctrl Pts',(27.7952841751738,1.49923165515646,3.9454531485941));
#24685=CARTESIAN_POINT('Ctrl Pts',(27.8167262899986,1.49645455657129,3.89372359169424));
#24686=CARTESIAN_POINT('Ctrl Pts',(27.832882321789,1.49448481141327,3.87013283011263));
#24687=CARTESIAN_POINT('Ctrl Pts',(27.870133075872,1.49077897157582,3.83288207602961));
#24688=CARTESIAN_POINT('Ctrl Pts',(27.8937237310949,1.48880073282317,3.81672623696367));
#24689=CARTESIAN_POINT('Ctrl Pts',(27.9454529259093,1.48600415954412,3.7952842627304));
#24690=CARTESIAN_POINT('Ctrl Pts',(27.9735944730755,1.48522725533839,3.79));
#24691=CARTESIAN_POINT('Ctrl Pts',(28.0264055269245,1.48522725533839,3.79));
#24692=CARTESIAN_POINT('Ctrl Pts',(28.0545470740907,1.48600415954412,3.7952842627304));
#24693=CARTESIAN_POINT('Ctrl Pts',(28.1062762689051,1.48880073282317,3.81672623696367));
#24694=CARTESIAN_POINT('Ctrl Pts',(28.129866924128,1.49077897157582,3.83288207602961));
#24695=CARTESIAN_POINT('Ctrl Pts',(28.167117678211,1.49448481141327,3.87013283011263));
#24696=CARTESIAN_POINT('Ctrl Pts',(28.1832737100014,1.49645455657129,3.89372359169424));
#24697=CARTESIAN_POINT('Ctrl Pts',(28.2047158248262,1.49923165515646,3.9454531485941));
#24698=CARTESIAN_POINT('Ctrl Pts',(28.21,1.5,3.97359482149072));
#24699=CARTESIAN_POINT('Ctrl Pts',(28.21,1.5,4.02640517850928));
#24700=CARTESIAN_POINT('Ctrl Pts',(28.2047158248262,1.49923165515646,4.0545468514059));
#24701=CARTESIAN_POINT('Ctrl Pts',(28.1832737100014,1.49645455657129,4.10627640830576));
#24702=CARTESIAN_POINT('Ctrl Pts',(28.167117678211,1.49448481141327,4.12986716988737));
#24703=CARTESIAN_POINT('Ctrl Pts',(28.129866924128,1.49077897157582,4.16711792397039));
#24704=CARTESIAN_POINT('Ctrl Pts',(28.1062762689051,1.48880073282317,4.18327376303633));
#24705=CARTESIAN_POINT('Ctrl Pts',(28.0545470740907,1.48600415954412,4.2047157372696));
#24706=CARTESIAN_POINT('Ctrl Pts',(28.0264055269245,1.48522725533839,4.21));
#24707=CARTESIAN_POINT('Ctrl Pts',(28.,1.48522725533839,4.21));
#24708=CARTESIAN_POINT('Origin',(28.,0.99,4.));
#24709=CARTESIAN_POINT('',(27.,0.99,3.85893264020334));
#24710=CARTESIAN_POINT('Origin',(26.9,-0.3,4.));
#24711=CARTESIAN_POINT('',(29.4,-0.3,2.5));
#24712=CARTESIAN_POINT('',(29.4,-0.3,3.04606079858305));
#24713=CARTESIAN_POINT('',(29.4,-0.3,4.));
#24714=CARTESIAN_POINT('',(28.8,-0.3,2.5));
#24715=CARTESIAN_POINT('',(26.9,-0.3,2.5));
#24716=CARTESIAN_POINT('',(28.8,-0.3,2.53030615433009));
#24717=CARTESIAN_POINT('',(28.8,-0.3,4.));
#24718=CARTESIAN_POINT('',(27.,-0.3,2.53030615433009));
#24719=CARTESIAN_POINT('',(27.,-0.3,2.53030615433009));
#24720=CARTESIAN_POINT('',(27.,-0.3,3.04606079858305));
#24721=CARTESIAN_POINT('',(27.,-0.3,4.));
#24722=CARTESIAN_POINT('',(27.,-0.3,3.04606079858305));
#24723=CARTESIAN_POINT('Origin',(26.9,-0.3,2.5));
#24724=CARTESIAN_POINT('',(29.4,0.3,2.5));
#24725=CARTESIAN_POINT('',(29.4,-0.15,2.5));
#24726=CARTESIAN_POINT('',(28.8,0.3,2.5));
#24727=CARTESIAN_POINT('',(26.9,0.3,2.5));
#24728=CARTESIAN_POINT('',(28.8,-0.15,2.5));
#24729=CARTESIAN_POINT('Origin',(26.9,0.3,2.5));
#24730=CARTESIAN_POINT('',(29.4,0.3,3.04606079858305));
#24731=CARTESIAN_POINT('',(29.4,0.3,3.25));
#24732=CARTESIAN_POINT('',(27.,0.3,3.04606079858305));
#24733=CARTESIAN_POINT('',(27.,0.3,3.04606079858305));
#24734=CARTESIAN_POINT('',(27.,0.3,2.53030615433009));
#24735=CARTESIAN_POINT('',(27.,0.3,3.25));
#24736=CARTESIAN_POINT('',(28.8,0.3,2.53030615433009));
#24737=CARTESIAN_POINT('',(27.,0.3,2.53030615433009));
#24738=CARTESIAN_POINT('',(28.8,0.3,3.25));
#24739=CARTESIAN_POINT('Origin',(29.4,0.,4.));
#24740=CARTESIAN_POINT('',(29.4,-4.28626379701574E-16,7.5));
#24741=CARTESIAN_POINT('Origin',(29.4,0.,4.));
#24742=CARTESIAN_POINT('Origin',(29.4,0.,4.));
#24743=CARTESIAN_POINT('Origin',(28.8,0.,4.));
#24744=CARTESIAN_POINT('',(28.8,-4.28626379701574E-16,7.5));
#24745=CARTESIAN_POINT('Origin',(28.8,0.,4.));
#24746=CARTESIAN_POINT('Origin',(28.8,0.,4.));
#24747=CARTESIAN_POINT('Origin',(28.8,0.,4.));
#24748=CARTESIAN_POINT('',(28.8,-4.28626379701574E-16,7.5));
#24749=CARTESIAN_POINT('Origin',(27.,0.,4.));
#24750=CARTESIAN_POINT('Origin',(27.,0.,4.));
#24751=CARTESIAN_POINT('Origin',(27.,0.,4.));
#24752=CARTESIAN_POINT('Origin',(27.,0.,4.));
#24753=CARTESIAN_POINT('Origin',(27.,0.,4.));
#24754=CARTESIAN_POINT('',(0.,0.,0.));
#24755=CARTESIAN_POINT('Origin',(29.4,0.,6.5));
#24756=CARTESIAN_POINT('',(31.03,-4.04133443718627E-17,6.83));
#24757=CARTESIAN_POINT('Origin',(31.03,0.,6.5));
#24758=CARTESIAN_POINT('',(29.4,-4.04133443718627E-17,6.83));
#24759=CARTESIAN_POINT('',(29.4,-4.04133443718627E-17,6.83));
#24760=CARTESIAN_POINT('Origin',(29.4,0.,6.5));
#24761=CARTESIAN_POINT('Origin',(29.4,0.,6.5));
#24762=CARTESIAN_POINT('',(31.03,-4.89858719658942E-17,6.9));
#24763=CARTESIAN_POINT('Origin',(31.03,0.,6.5));
#24764=CARTESIAN_POINT('',(29.4,-4.89858719658942E-17,6.9));
#24765=CARTESIAN_POINT('',(29.4,-4.89858719658942E-17,6.9));
#24766=CARTESIAN_POINT('Origin',(29.4,0.,6.5));
#24767=CARTESIAN_POINT('Origin',(31.03,0.,6.5));
#24768=CARTESIAN_POINT('Origin',(29.4,0.,6.5));
#24769=CARTESIAN_POINT('',(0.,0.,0.));
#24770=CARTESIAN_POINT('Origin',(29.4,0.,6.5));
#24771=CARTESIAN_POINT('',(31.,-4.95981953654678E-17,6.905));
#24772=CARTESIAN_POINT('Origin',(31.,0.,6.5));
#24773=CARTESIAN_POINT('',(29.4,-4.95981953654678E-17,6.905));
#24774=CARTESIAN_POINT('',(29.4,-4.95981953654678E-17,6.905));
#24775=CARTESIAN_POINT('Origin',(29.4,0.,6.5));
#24776=CARTESIAN_POINT('Origin',(29.4,0.,6.5));
#24777=CARTESIAN_POINT('',(31.,-1.10218211923262E-16,7.4));
#24778=CARTESIAN_POINT('Origin',(31.,0.,6.5));
#24779=CARTESIAN_POINT('',(29.4,-1.10218211923262E-16,7.4));
#24780=CARTESIAN_POINT('',(29.4,-1.10218211923262E-16,7.4));
#24781=CARTESIAN_POINT('Origin',(29.4,0.,6.5));
#24782=CARTESIAN_POINT('Origin',(31.,0.,6.5));
#24783=CARTESIAN_POINT('Origin',(29.4,0.,6.5));
#24784=CARTESIAN_POINT('',(0.,0.,0.));
#24785=CARTESIAN_POINT('Origin',(-1.,0.,0.35));
#24786=CARTESIAN_POINT('',(-1.,-0.26,0.6));
#24787=CARTESIAN_POINT('',(-1.,-0.3,0.56));
#24788=CARTESIAN_POINT('',(-1.,-0.2675,0.5925));
#24789=CARTESIAN_POINT('',(-1.,0.26,0.6));
#24790=CARTESIAN_POINT('',(-1.,0.,0.6));
#24791=CARTESIAN_POINT('',(-1.,0.3,0.56));
#24792=CARTESIAN_POINT('',(-1.,0.2675,0.5925));
#24793=CARTESIAN_POINT('',(-1.,0.3,0.04));
#24794=CARTESIAN_POINT('',(-1.,0.3,0.175));
#24795=CARTESIAN_POINT('',(-1.,0.26,0.));
#24796=CARTESIAN_POINT('',(-1.,0.2925,0.0325));
#24797=CARTESIAN_POINT('',(-1.,-0.26,0.));
#24798=CARTESIAN_POINT('',(-1.,0.,0.));
#24799=CARTESIAN_POINT('',(-1.,-0.3,0.04));
#24800=CARTESIAN_POINT('',(-1.,-0.2925,0.0325));
#24801=CARTESIAN_POINT('',(-1.,-0.3,0.175));
#24802=CARTESIAN_POINT('Origin',(0.75,0.28,0.02));
#24803=CARTESIAN_POINT('',(1.,0.3,0.04));
#24804=CARTESIAN_POINT('',(0.75,0.3,0.04));
#24805=CARTESIAN_POINT('',(1.,0.26,0.));
#24806=CARTESIAN_POINT('',(1.,0.2925,0.0325));
#24807=CARTESIAN_POINT('',(0.75,0.26,0.));
#24808=CARTESIAN_POINT('Origin',(1.5,0.3,0.));
#24809=CARTESIAN_POINT('',(1.,0.3,0.56));
#24810=CARTESIAN_POINT('',(0.75,0.3,0.56));
#24811=CARTESIAN_POINT('',(1.,0.3,0.175));
#24812=CARTESIAN_POINT('Origin',(0.75,0.28,0.58));
#24813=CARTESIAN_POINT('',(1.,0.26,0.6));
#24814=CARTESIAN_POINT('',(0.75,0.26,0.6));
#24815=CARTESIAN_POINT('',(1.,0.2675,0.5925));
#24816=CARTESIAN_POINT('Origin',(0.,0.,0.6));
#24817=CARTESIAN_POINT('',(1.,-0.26,0.6));
#24818=CARTESIAN_POINT('',(-0.75,-0.26,0.6));
#24819=CARTESIAN_POINT('',(1.,0.,0.6));
#24820=CARTESIAN_POINT('Origin',(1.,0.,0.35));
#24821=CARTESIAN_POINT('',(1.,-0.26,0.));
#24822=CARTESIAN_POINT('',(1.,-0.3,0.04));
#24823=CARTESIAN_POINT('',(1.,-0.2925,0.0325));
#24824=CARTESIAN_POINT('',(1.,0.,0.));
#24825=CARTESIAN_POINT('',(1.,-0.3,0.56));
#24826=CARTESIAN_POINT('',(1.,-0.2675,0.5925));
#24827=CARTESIAN_POINT('',(1.,-0.3,0.175));
#24828=CARTESIAN_POINT('Origin',(0.,0.,0.));
#24829=CARTESIAN_POINT('',(-0.75,-0.26,0.));
#24830=CARTESIAN_POINT('Origin',(-0.75,-0.28,0.58));
#24831=CARTESIAN_POINT('',(-0.75,-0.3,0.56));
#24832=CARTESIAN_POINT('Origin',(-0.75,-0.28,0.02));
#24833=CARTESIAN_POINT('',(-0.75,-0.3,0.04));
#24834=CARTESIAN_POINT('Origin',(-1.5,-0.3,0.));
#24835=CARTESIAN_POINT('',(0.,0.,0.));
#24836=CARTESIAN_POINT('Origin',(0.0721687836487032,0.,-0.125));
#24837=CARTESIAN_POINT('',(0.0721687836487032,0.,-0.125));
#24838=CARTESIAN_POINT('',(0.144337567297406,0.,0.));
#24839=CARTESIAN_POINT('',(0.117710979560879,0.,-0.0461186027918559));
#24840=CARTESIAN_POINT('',(0.0721687836487032,-0.25,-0.125));
#24841=CARTESIAN_POINT('',(0.0721687836487032,0.,-0.125));
#24842=CARTESIAN_POINT('',(0.144337567297406,-0.25,0.));
#24843=CARTESIAN_POINT('',(0.144337567297406,-0.25,0.));
#24844=CARTESIAN_POINT('',(0.144337567297406,0.,0.));
#24845=CARTESIAN_POINT('Origin',(-0.0721687836487032,0.,-0.125));
#24846=CARTESIAN_POINT('',(-0.0721687836487032,0.,-0.125));
#24847=CARTESIAN_POINT('',(0.0739156081756484,0.,-0.125));
#24848=CARTESIAN_POINT('',(-0.0721687836487032,-0.25,-0.125));
#24849=CARTESIAN_POINT('',(-0.0721687836487032,0.,-0.125));
#24850=CARTESIAN_POINT('',(0.0721687836487032,-0.25,-0.125));
#24851=CARTESIAN_POINT('Origin',(-0.144337567297406,0.,-4.16333634234434E-17));
#24852=CARTESIAN_POINT('',(-0.144337567297406,0.,-1.76762539787485E-17));
#24853=CARTESIAN_POINT('',(-0.0987953713852306,0.,-0.0788813972081442));
#24854=CARTESIAN_POINT('',(-0.144337567297406,-0.25,-2.77555756156289E-17));
#24855=CARTESIAN_POINT('',(-0.144337567297406,0.,-1.76762539787485E-17));
#24856=CARTESIAN_POINT('',(-0.0721687836487032,-0.25,-0.125));
#24857=CARTESIAN_POINT('Origin',(-0.0721687836487033,0.,0.125));
#24858=CARTESIAN_POINT('',(-0.0721687836487033,0.,0.125));
#24859=CARTESIAN_POINT('',(-0.0627109795608791,0.,0.141381397208144));
#24860=CARTESIAN_POINT('',(-0.0721687836487033,-0.25,0.125));
#24861=CARTESIAN_POINT('',(-0.0721687836487033,0.,0.125));
#24862=CARTESIAN_POINT('',(-0.144337567297406,-0.25,-1.76762539787485E-17));
#24863=CARTESIAN_POINT('Origin',(0.0721687836487032,0.,0.125));
#24864=CARTESIAN_POINT('',(0.0721687836487032,0.,0.125));
#24865=CARTESIAN_POINT('',(0.146084391824352,0.,0.125));
#24866=CARTESIAN_POINT('',(0.0721687836487032,-0.25,0.125));
#24867=CARTESIAN_POINT('',(0.0721687836487032,0.,0.125));
#24868=CARTESIAN_POINT('',(-0.0721687836487033,-0.25,0.125));
#24869=CARTESIAN_POINT('Origin',(0.144337567297406,0.,0.));
#24870=CARTESIAN_POINT('',(0.153795371385231,0.,-0.0163813972081441));
#24871=CARTESIAN_POINT('',(0.0721687836487032,-0.25,0.125));
#24872=CARTESIAN_POINT('Origin',(0.,-0.25,0.));
#24873=CARTESIAN_POINT('Origin',(0.22,0.,0.));
#24874=CARTESIAN_POINT('',(-0.22,-8.67361737988404E-18,-2.69422295812418E-17));
#24875=CARTESIAN_POINT('Origin',(0.,0.,0.));
#24876=CARTESIAN_POINT('Origin',(0.,-0.015,0.));
#24877=CARTESIAN_POINT('',(-0.24505,-0.02505,-3.00099698131059E-17));
#24878=CARTESIAN_POINT('Origin',(0.,-0.02505,0.));
#24879=CARTESIAN_POINT('',(-0.235,-0.015,-2.87791997799628E-17));
#24880=CARTESIAN_POINT('Origin',(0.,-0.3775,0.));
#24881=CARTESIAN_POINT('',(-0.24505,-0.72995,3.00099698131059E-17));
#24882=CARTESIAN_POINT('Origin',(0.,-0.72995,0.));
#24883=CARTESIAN_POINT('',(-0.24505,-0.3775,-3.00099698131059E-17));
#24884=CARTESIAN_POINT('Origin',(0.,-0.7625,0.));
#24885=CARTESIAN_POINT('',(-0.175,-0.8,-2.14313189850787E-17));
#24886=CARTESIAN_POINT('Origin',(0.,-0.8,0.));
#24887=CARTESIAN_POINT('',(-0.2125,-0.7625,-2.60237444818813E-17));
#24888=CARTESIAN_POINT('Origin',(0.,-0.8,0.));
#24889=CARTESIAN_POINT('',(0.,0.,0.));
#24890=CARTESIAN_POINT('Origin',(0.,0.,0.));
#24891=CARTESIAN_POINT('',(-0.32,0.16,3.91886975727153E-17));
#24892=CARTESIAN_POINT('Origin',(0.,0.16,0.));
#24893=CARTESIAN_POINT('',(-0.32,0.,3.91886975727153E-17));
#24894=CARTESIAN_POINT('',(-0.32,0.,3.91886975727153E-17));
#24895=CARTESIAN_POINT('Origin',(0.,0.,0.));
#24896=CARTESIAN_POINT('Origin',(0.,0.,0.));
#24897=CARTESIAN_POINT('',(-0.6,0.16,7.34788079488412E-17));
#24898=CARTESIAN_POINT('Origin',(0.,0.16,0.));
#24899=CARTESIAN_POINT('',(-0.6,0.,7.34788079488412E-17));
#24900=CARTESIAN_POINT('',(-0.6,0.,7.34788079488412E-17));
#24901=CARTESIAN_POINT('Origin',(0.,0.,0.));
#24902=CARTESIAN_POINT('Origin',(0.,0.16,0.));
#24903=CARTESIAN_POINT('Origin',(0.,0.,0.));
#24904=CARTESIAN_POINT('',(0.,0.,0.));
#24905=CARTESIAN_POINT('Origin',(0.45,0.6,0.));
#24906=CARTESIAN_POINT('',(-0.45,0.6,-5.51091059616309E-17));
#24907=CARTESIAN_POINT('Origin',(0.,0.6,0.));
#24908=CARTESIAN_POINT('Origin',(0.,0.575,0.));
#24909=CARTESIAN_POINT('',(-0.5,0.55,-6.12323399573677E-17));
#24910=CARTESIAN_POINT('Origin',(0.,0.55,0.));
#24911=CARTESIAN_POINT('',(-0.475,0.575,-5.81707229594993E-17));
#24912=CARTESIAN_POINT('Origin',(0.,0.29,0.));
#24913=CARTESIAN_POINT('',(-0.5,0.0299999999999998,-6.12323399573677E-17));
#24914=CARTESIAN_POINT('Origin',(0.,0.0299999999999998,0.));
#24915=CARTESIAN_POINT('',(-0.5,0.29,-6.12323399573677E-17));
#24916=CARTESIAN_POINT('Origin',(0.,0.0150000000000001,0.));
#24917=CARTESIAN_POINT('',(-0.47,7.11236625150491E-17,-5.75583995599256E-17));
#24918=CARTESIAN_POINT('Origin',(0.,0.,0.));
#24919=CARTESIAN_POINT('',(-0.485,0.0150000000000001,-5.93953697586466E-17));
#24920=CARTESIAN_POINT('Origin',(0.32,0.,0.));
#24921=CARTESIAN_POINT('',(-0.32,-6.93889390390723E-18,-3.91886975727153E-17));
#24922=CARTESIAN_POINT('Origin',(0.,0.,0.));
#24923=CARTESIAN_POINT('Origin',(0.,-0.02,0.));
#24924=CARTESIAN_POINT('',(-0.2942,-0.0515999999999999,3.60291088309151E-17));
#24925=CARTESIAN_POINT('Origin',(0.,-0.0515999999999999,0.));
#24926=CARTESIAN_POINT('',(-0.31,-0.02,-3.7964050773568E-17));
#24927=CARTESIAN_POINT('Origin',(0.,-1.24,0.));
#24928=CARTESIAN_POINT('',(-0.2942,-2.4458,3.60291088309151E-17));
#24929=CARTESIAN_POINT('Origin',(0.,-2.4458,0.));
#24930=CARTESIAN_POINT('',(-0.2942,-1.24,-3.60291088309151E-17));
#24931=CARTESIAN_POINT('Origin',(0.,-2.47,0.));
#24932=CARTESIAN_POINT('',(-0.24,-2.5,-2.93915231795365E-17));
#24933=CARTESIAN_POINT('Origin',(0.,-2.5,0.));
#24934=CARTESIAN_POINT('',(-0.27,-2.47,-3.30654635769785E-17));
#24935=CARTESIAN_POINT('Origin',(0.,-2.5,0.));
#24936=CARTESIAN_POINT('Origin',(0.144337567297406,-0.6,-0.25));
#24937=CARTESIAN_POINT('',(0.288675134594813,-0.6,0.));
#24938=CARTESIAN_POINT('',(0.144337567297406,-0.6,-0.25));
#24939=CARTESIAN_POINT('',(0.288675134594813,-0.6,0.));
#24940=CARTESIAN_POINT('',(0.144337567297406,-0.96,-0.25));
#24941=CARTESIAN_POINT('',(0.144337567297406,-0.6,-0.25));
#24942=CARTESIAN_POINT('',(0.288675134594813,-0.96,0.));
#24943=CARTESIAN_POINT('',(0.288675134594813,-0.96,0.));
#24944=CARTESIAN_POINT('',(0.288675134594813,-0.6,0.));
#24945=CARTESIAN_POINT('Origin',(-0.144337567297406,-0.6,-0.25));
#24946=CARTESIAN_POINT('',(-0.144337567297406,-0.6,-0.25));
#24947=CARTESIAN_POINT('',(0.144337567297406,-0.6,-0.25));
#24948=CARTESIAN_POINT('',(-0.144337567297406,-0.96,-0.25));
#24949=CARTESIAN_POINT('',(-0.144337567297406,-0.6,-0.25));
#24950=CARTESIAN_POINT('',(0.144337567297406,-0.96,-0.25));
#24951=CARTESIAN_POINT('Origin',(-0.288675134594813,-0.6,-8.32667268468867E-17));
#24952=CARTESIAN_POINT('',(-0.288675134594813,-0.6,-3.53525079574969E-17));
#24953=CARTESIAN_POINT('',(-0.144337567297406,-0.6,-0.25));
#24954=CARTESIAN_POINT('',(-0.288675134594813,-0.96,-5.55111512312578E-17));
#24955=CARTESIAN_POINT('',(-0.288675134594813,-0.6,-3.53525079574969E-17));
#24956=CARTESIAN_POINT('',(-0.144337567297406,-0.96,-0.25));
#24957=CARTESIAN_POINT('Origin',(-0.144337567297407,-0.6,0.25));
#24958=CARTESIAN_POINT('',(-0.144337567297407,-0.6,0.25));
#24959=CARTESIAN_POINT('',(-0.288675134594813,-0.6,-3.53525079574969E-17));
#24960=CARTESIAN_POINT('',(-0.144337567297407,-0.96,0.25));
#24961=CARTESIAN_POINT('',(-0.144337567297407,-0.6,0.25));
#24962=CARTESIAN_POINT('',(-0.288675134594813,-0.96,-3.53525079574969E-17));
#24963=CARTESIAN_POINT('Origin',(0.144337567297406,-0.6,0.25));
#24964=CARTESIAN_POINT('',(0.144337567297406,-0.6,0.25));
#24965=CARTESIAN_POINT('',(-0.144337567297407,-0.6,0.25));
#24966=CARTESIAN_POINT('',(0.144337567297406,-0.96,0.25));
#24967=CARTESIAN_POINT('',(0.144337567297406,-0.6,0.25));
#24968=CARTESIAN_POINT('',(-0.144337567297407,-0.96,0.25));
#24969=CARTESIAN_POINT('Origin',(0.288675134594813,-0.6,0.));
#24970=CARTESIAN_POINT('',(0.144337567297406,-0.6,0.25));
#24971=CARTESIAN_POINT('',(0.144337567297406,-0.96,0.25));
#24972=CARTESIAN_POINT('Origin',(0.,-0.6,0.));
#24973=CARTESIAN_POINT('Origin',(0.,-0.96,0.));
#24974=CARTESIAN_POINT('',(0.,0.,0.));
#24975=CARTESIAN_POINT('',(0.,0.,0.));
#24976=CARTESIAN_POINT('',(0.,0.,0.));
#24977=CARTESIAN_POINT('',(0.,0.,0.));
#24978=CARTESIAN_POINT('',(0.,0.,0.));
#24979=CARTESIAN_POINT('',(0.,0.,0.));
#24980=CARTESIAN_POINT('',(5.,0.,0.));
#24981=CARTESIAN_POINT('',(11.,0.,0.));
#24982=CARTESIAN_POINT('',(18.,0.,0.));
#24983=CARTESIAN_POINT('',(1.5,-3.5,0.));
#24984=CARTESIAN_POINT('',(1.5,3.5,0.));
#24985=CARTESIAN_POINT('',(24.,-3.5,0.));
#24986=CARTESIAN_POINT('',(24.,3.5,0.));
#24987=CARTESIAN_POINT('',(24.,0.,4.));
#24988=CARTESIAN_POINT('',(25.4,2.6,4.));
#24989=CARTESIAN_POINT('',(25.4,4.44089209850063E-16,6.6));
#24990=CARTESIAN_POINT('',(25.4,-2.6,4.));
#24991=CARTESIAN_POINT('',(3.45,-3.,5.8));
#24992=CARTESIAN_POINT('',(3.45,3.,5.8));
#24993=CARTESIAN_POINT('',(0.,0.,0.));
#24994=CARTESIAN_POINT('',(0.,0.,0.));
#24995=CARTESIAN_POINT('',(0.,0.,0.));
#24996=CARTESIAN_POINT('',(0.,0.,0.));
#24997=CARTESIAN_POINT('',(0.,0.,0.));
#24998=CARTESIAN_POINT('',(-1.10423359219112E-15,6.47281095066036,7.09390099933374));
#24999=CARTESIAN_POINT('',(25.8,1.8,4.));
#25000=CARTESIAN_POINT('',(28.2,0.,3.35));
#25001=CARTESIAN_POINT('',(28.,1.8,4.));
#25002=CARTESIAN_POINT('',(31.03,0.,6.5));
#25003=CARTESIAN_POINT('',(31.19,0.,6.5));
#25004=CARTESIAN_POINT('',(0.,0.,0.));
#25005=CARTESIAN_POINT('',(-1.10023051629276,-1.09296832172218E-61,1.33226762955019E-15));
#25006=CARTESIAN_POINT('',(1.18094038521554E-16,3.45440543675711,6.01670103845455));
#25007=UNCERTAINTY_MEASURE_WITH_UNIT(LENGTH_MEASURE(0.001),#25075,
'DISTANCE_ACCURACY_VALUE',
'Maximum model space distance between geometric entities at asserted c
onnectivities');
#25008=UNCERTAINTY_MEASURE_WITH_UNIT(LENGTH_MEASURE(0.001),#25075,
'DISTANCE_ACCURACY_VALUE',
'Maximum model space distance between geometric entities at asserted c
onnectivities');
#25009=UNCERTAINTY_MEASURE_WITH_UNIT(LENGTH_MEASURE(0.001),#25075,
'DISTANCE_ACCURACY_VALUE',
'Maximum model space distance between geometric entities at asserted c
onnectivities');
#25010=UNCERTAINTY_MEASURE_WITH_UNIT(LENGTH_MEASURE(0.001),#25075,
'DISTANCE_ACCURACY_VALUE',
'Maximum model space distance between geometric entities at asserted c
onnectivities');
#25011=UNCERTAINTY_MEASURE_WITH_UNIT(LENGTH_MEASURE(0.001),#25075,
'DISTANCE_ACCURACY_VALUE',
'Maximum model space distance between geometric entities at asserted c
onnectivities');
#25012=UNCERTAINTY_MEASURE_WITH_UNIT(LENGTH_MEASURE(0.001),#25075,
'DISTANCE_ACCURACY_VALUE',
'Maximum model space distance between geometric entities at asserted c
onnectivities');
#25013=UNCERTAINTY_MEASURE_WITH_UNIT(LENGTH_MEASURE(0.001),#25075,
'DISTANCE_ACCURACY_VALUE',
'Maximum model space distance between geometric entities at asserted c
onnectivities');
#25014=UNCERTAINTY_MEASURE_WITH_UNIT(LENGTH_MEASURE(0.001),#25075,
'DISTANCE_ACCURACY_VALUE',
'Maximum model space distance between geometric entities at asserted c
onnectivities');
#25015=UNCERTAINTY_MEASURE_WITH_UNIT(LENGTH_MEASURE(0.001),#25075,
'DISTANCE_ACCURACY_VALUE',
'Maximum model space distance between geometric entities at asserted c
onnectivities');
#25016=UNCERTAINTY_MEASURE_WITH_UNIT(LENGTH_MEASURE(0.001),#25075,
'DISTANCE_ACCURACY_VALUE',
'Maximum model space distance between geometric entities at asserted c
onnectivities');
#25017=UNCERTAINTY_MEASURE_WITH_UNIT(LENGTH_MEASURE(0.001),#25075,
'DISTANCE_ACCURACY_VALUE',
'Maximum model space distance between geometric entities at asserted c
onnectivities');
#25018=UNCERTAINTY_MEASURE_WITH_UNIT(LENGTH_MEASURE(0.001),#25075,
'DISTANCE_ACCURACY_VALUE',
'Maximum model space distance between geometric entities at asserted c
onnectivities');
#25019=UNCERTAINTY_MEASURE_WITH_UNIT(LENGTH_MEASURE(0.001),#25075,
'DISTANCE_ACCURACY_VALUE',
'Maximum model space distance between geometric entities at asserted c
onnectivities');
#25020=UNCERTAINTY_MEASURE_WITH_UNIT(LENGTH_MEASURE(0.001),#25075,
'DISTANCE_ACCURACY_VALUE',
'Maximum model space distance between geometric entities at asserted c
onnectivities');
#25021=UNCERTAINTY_MEASURE_WITH_UNIT(LENGTH_MEASURE(0.001),#25075,
'DISTANCE_ACCURACY_VALUE',
'Maximum model space distance between geometric entities at asserted c
onnectivities');
#25022=UNCERTAINTY_MEASURE_WITH_UNIT(LENGTH_MEASURE(0.001),#25075,
'DISTANCE_ACCURACY_VALUE',
'Maximum model space distance between geometric entities at asserted c
onnectivities');
#25023=UNCERTAINTY_MEASURE_WITH_UNIT(LENGTH_MEASURE(0.001),#25075,
'DISTANCE_ACCURACY_VALUE',
'Maximum model space distance between geometric entities at asserted c
onnectivities');
#25024=UNCERTAINTY_MEASURE_WITH_UNIT(LENGTH_MEASURE(0.001),#25075,
'DISTANCE_ACCURACY_VALUE',
'Maximum model space distance between geometric entities at asserted c
onnectivities');
#25025=UNCERTAINTY_MEASURE_WITH_UNIT(LENGTH_MEASURE(0.001),#25075,
'DISTANCE_ACCURACY_VALUE',
'Maximum model space distance between geometric entities at asserted c
onnectivities');
#25026=UNCERTAINTY_MEASURE_WITH_UNIT(LENGTH_MEASURE(0.001),#25075,
'DISTANCE_ACCURACY_VALUE',
'Maximum model space distance between geometric entities at asserted c
onnectivities');
#25027=UNCERTAINTY_MEASURE_WITH_UNIT(LENGTH_MEASURE(0.001),#25075,
'DISTANCE_ACCURACY_VALUE',
'Maximum model space distance between geometric entities at asserted c
onnectivities');
#25028=UNCERTAINTY_MEASURE_WITH_UNIT(LENGTH_MEASURE(0.001),#25075,
'DISTANCE_ACCURACY_VALUE',
'Maximum model space distance between geometric entities at asserted c
onnectivities');
#25029=UNCERTAINTY_MEASURE_WITH_UNIT(LENGTH_MEASURE(0.001),#25075,
'DISTANCE_ACCURACY_VALUE',
'Maximum model space distance between geometric entities at asserted c
onnectivities');
#25030=UNCERTAINTY_MEASURE_WITH_UNIT(LENGTH_MEASURE(0.001),#25075,
'DISTANCE_ACCURACY_VALUE',
'Maximum model space distance between geometric entities at asserted c
onnectivities');
#25031=UNCERTAINTY_MEASURE_WITH_UNIT(LENGTH_MEASURE(0.001),#25075,
'DISTANCE_ACCURACY_VALUE',
'Maximum model space distance between geometric entities at asserted c
onnectivities');
#25032=UNCERTAINTY_MEASURE_WITH_UNIT(LENGTH_MEASURE(0.001),#25075,
'DISTANCE_ACCURACY_VALUE',
'Maximum model space distance between geometric entities at asserted c
onnectivities');
#25033=UNCERTAINTY_MEASURE_WITH_UNIT(LENGTH_MEASURE(0.001),#25075,
'DISTANCE_ACCURACY_VALUE',
'Maximum model space distance between geometric entities at asserted c
onnectivities');
#25034=UNCERTAINTY_MEASURE_WITH_UNIT(LENGTH_MEASURE(0.001),#25075,
'DISTANCE_ACCURACY_VALUE',
'Maximum model space distance between geometric entities at asserted c
onnectivities');
#25035=UNCERTAINTY_MEASURE_WITH_UNIT(LENGTH_MEASURE(0.001),#25075,
'DISTANCE_ACCURACY_VALUE',
'Maximum model space distance between geometric entities at asserted c
onnectivities');
#25036=UNCERTAINTY_MEASURE_WITH_UNIT(LENGTH_MEASURE(0.001),#25075,
'DISTANCE_ACCURACY_VALUE',
'Maximum model space distance between geometric entities at asserted c
onnectivities');
#25037=UNCERTAINTY_MEASURE_WITH_UNIT(LENGTH_MEASURE(0.001),#25075,
'DISTANCE_ACCURACY_VALUE',
'Maximum model space distance between geometric entities at asserted c
onnectivities');
#25038=UNCERTAINTY_MEASURE_WITH_UNIT(LENGTH_MEASURE(0.001),#25075,
'DISTANCE_ACCURACY_VALUE',
'Maximum model space distance between geometric entities at asserted c
onnectivities');
#25039=UNCERTAINTY_MEASURE_WITH_UNIT(LENGTH_MEASURE(0.001),#25075,
'DISTANCE_ACCURACY_VALUE',
'Maximum model space distance between geometric entities at asserted c
onnectivities');
#25040=UNCERTAINTY_MEASURE_WITH_UNIT(LENGTH_MEASURE(0.001),#25075,
'DISTANCE_ACCURACY_VALUE',
'Maximum model space distance between geometric entities at asserted c
onnectivities');
#25041=(
GEOMETRIC_REPRESENTATION_CONTEXT(3)
GLOBAL_UNCERTAINTY_ASSIGNED_CONTEXT((#25007))
GLOBAL_UNIT_ASSIGNED_CONTEXT((#25075,#25077,#25078))
REPRESENTATION_CONTEXT('','3D')
);
#25042=(
GEOMETRIC_REPRESENTATION_CONTEXT(3)
GLOBAL_UNCERTAINTY_ASSIGNED_CONTEXT((#25008))
GLOBAL_UNIT_ASSIGNED_CONTEXT((#25075,#25077,#25078))
REPRESENTATION_CONTEXT('','3D')
);
#25043=(
GEOMETRIC_REPRESENTATION_CONTEXT(3)
GLOBAL_UNCERTAINTY_ASSIGNED_CONTEXT((#25009))
GLOBAL_UNIT_ASSIGNED_CONTEXT((#25075,#25077,#25078))
REPRESENTATION_CONTEXT('','3D')
);
#25044=(
GEOMETRIC_REPRESENTATION_CONTEXT(3)
GLOBAL_UNCERTAINTY_ASSIGNED_CONTEXT((#25010))
GLOBAL_UNIT_ASSIGNED_CONTEXT((#25075,#25077,#25078))
REPRESENTATION_CONTEXT('','3D')
);
#25045=(
GEOMETRIC_REPRESENTATION_CONTEXT(3)
GLOBAL_UNCERTAINTY_ASSIGNED_CONTEXT((#25011))
GLOBAL_UNIT_ASSIGNED_CONTEXT((#25075,#25077,#25078))
REPRESENTATION_CONTEXT('','3D')
);
#25046=(
GEOMETRIC_REPRESENTATION_CONTEXT(3)
GLOBAL_UNCERTAINTY_ASSIGNED_CONTEXT((#25012))
GLOBAL_UNIT_ASSIGNED_CONTEXT((#25075,#25077,#25078))
REPRESENTATION_CONTEXT('','3D')
);
#25047=(
GEOMETRIC_REPRESENTATION_CONTEXT(3)
GLOBAL_UNCERTAINTY_ASSIGNED_CONTEXT((#25013))
GLOBAL_UNIT_ASSIGNED_CONTEXT((#25075,#25077,#25078))
REPRESENTATION_CONTEXT('','3D')
);
#25048=(
GEOMETRIC_REPRESENTATION_CONTEXT(3)
GLOBAL_UNCERTAINTY_ASSIGNED_CONTEXT((#25014))
GLOBAL_UNIT_ASSIGNED_CONTEXT((#25075,#25077,#25078))
REPRESENTATION_CONTEXT('','3D')
);
#25049=(
GEOMETRIC_REPRESENTATION_CONTEXT(3)
GLOBAL_UNCERTAINTY_ASSIGNED_CONTEXT((#25015))
GLOBAL_UNIT_ASSIGNED_CONTEXT((#25075,#25077,#25078))
REPRESENTATION_CONTEXT('','3D')
);
#25050=(
GEOMETRIC_REPRESENTATION_CONTEXT(3)
GLOBAL_UNCERTAINTY_ASSIGNED_CONTEXT((#25016))
GLOBAL_UNIT_ASSIGNED_CONTEXT((#25075,#25077,#25078))
REPRESENTATION_CONTEXT('','3D')
);
#25051=(
GEOMETRIC_REPRESENTATION_CONTEXT(3)
GLOBAL_UNCERTAINTY_ASSIGNED_CONTEXT((#25017))
GLOBAL_UNIT_ASSIGNED_CONTEXT((#25075,#25077,#25078))
REPRESENTATION_CONTEXT('','3D')
);
#25052=(
GEOMETRIC_REPRESENTATION_CONTEXT(3)
GLOBAL_UNCERTAINTY_ASSIGNED_CONTEXT((#25018))
GLOBAL_UNIT_ASSIGNED_CONTEXT((#25075,#25077,#25078))
REPRESENTATION_CONTEXT('','3D')
);
#25053=(
GEOMETRIC_REPRESENTATION_CONTEXT(3)
GLOBAL_UNCERTAINTY_ASSIGNED_CONTEXT((#25019))
GLOBAL_UNIT_ASSIGNED_CONTEXT((#25075,#25077,#25078))
REPRESENTATION_CONTEXT('','3D')
);
#25054=(
GEOMETRIC_REPRESENTATION_CONTEXT(3)
GLOBAL_UNCERTAINTY_ASSIGNED_CONTEXT((#25020))
GLOBAL_UNIT_ASSIGNED_CONTEXT((#25075,#25077,#25078))
REPRESENTATION_CONTEXT('','3D')
);
#25055=(
GEOMETRIC_REPRESENTATION_CONTEXT(3)
GLOBAL_UNCERTAINTY_ASSIGNED_CONTEXT((#25021))
GLOBAL_UNIT_ASSIGNED_CONTEXT((#25075,#25077,#25078))
REPRESENTATION_CONTEXT('','3D')
);
#25056=(
GEOMETRIC_REPRESENTATION_CONTEXT(3)
GLOBAL_UNCERTAINTY_ASSIGNED_CONTEXT((#25022))
GLOBAL_UNIT_ASSIGNED_CONTEXT((#25075,#25077,#25078))
REPRESENTATION_CONTEXT('','3D')
);
#25057=(
GEOMETRIC_REPRESENTATION_CONTEXT(3)
GLOBAL_UNCERTAINTY_ASSIGNED_CONTEXT((#25023))
GLOBAL_UNIT_ASSIGNED_CONTEXT((#25075,#25077,#25078))
REPRESENTATION_CONTEXT('','3D')
);
#25058=(
GEOMETRIC_REPRESENTATION_CONTEXT(3)
GLOBAL_UNCERTAINTY_ASSIGNED_CONTEXT((#25024))
GLOBAL_UNIT_ASSIGNED_CONTEXT((#25075,#25077,#25078))
REPRESENTATION_CONTEXT('','3D')
);
#25059=(
GEOMETRIC_REPRESENTATION_CONTEXT(3)
GLOBAL_UNCERTAINTY_ASSIGNED_CONTEXT((#25025))
GLOBAL_UNIT_ASSIGNED_CONTEXT((#25075,#25077,#25078))
REPRESENTATION_CONTEXT('','3D')
);
#25060=(
GEOMETRIC_REPRESENTATION_CONTEXT(3)
GLOBAL_UNCERTAINTY_ASSIGNED_CONTEXT((#25026))
GLOBAL_UNIT_ASSIGNED_CONTEXT((#25075,#25077,#25078))
REPRESENTATION_CONTEXT('','3D')
);
#25061=(
GEOMETRIC_REPRESENTATION_CONTEXT(3)
GLOBAL_UNCERTAINTY_ASSIGNED_CONTEXT((#25027))
GLOBAL_UNIT_ASSIGNED_CONTEXT((#25075,#25077,#25078))
REPRESENTATION_CONTEXT('','3D')
);
#25062=(
GEOMETRIC_REPRESENTATION_CONTEXT(3)
GLOBAL_UNCERTAINTY_ASSIGNED_CONTEXT((#25028))
GLOBAL_UNIT_ASSIGNED_CONTEXT((#25075,#25077,#25078))
REPRESENTATION_CONTEXT('','3D')
);
#25063=(
GEOMETRIC_REPRESENTATION_CONTEXT(3)
GLOBAL_UNCERTAINTY_ASSIGNED_CONTEXT((#25029))
GLOBAL_UNIT_ASSIGNED_CONTEXT((#25075,#25077,#25078))
REPRESENTATION_CONTEXT('','3D')
);
#25064=(
GEOMETRIC_REPRESENTATION_CONTEXT(3)
GLOBAL_UNCERTAINTY_ASSIGNED_CONTEXT((#25030))
GLOBAL_UNIT_ASSIGNED_CONTEXT((#25075,#25077,#25078))
REPRESENTATION_CONTEXT('','3D')
);
#25065=(
GEOMETRIC_REPRESENTATION_CONTEXT(3)
GLOBAL_UNCERTAINTY_ASSIGNED_CONTEXT((#25031))
GLOBAL_UNIT_ASSIGNED_CONTEXT((#25075,#25077,#25078))
REPRESENTATION_CONTEXT('','3D')
);
#25066=(
GEOMETRIC_REPRESENTATION_CONTEXT(3)
GLOBAL_UNCERTAINTY_ASSIGNED_CONTEXT((#25032))
GLOBAL_UNIT_ASSIGNED_CONTEXT((#25075,#25077,#25078))
REPRESENTATION_CONTEXT('','3D')
);
#25067=(
GEOMETRIC_REPRESENTATION_CONTEXT(3)
GLOBAL_UNCERTAINTY_ASSIGNED_CONTEXT((#25033))
GLOBAL_UNIT_ASSIGNED_CONTEXT((#25075,#25077,#25078))
REPRESENTATION_CONTEXT('','3D')
);
#25068=(
GEOMETRIC_REPRESENTATION_CONTEXT(3)
GLOBAL_UNCERTAINTY_ASSIGNED_CONTEXT((#25034))
GLOBAL_UNIT_ASSIGNED_CONTEXT((#25075,#25077,#25078))
REPRESENTATION_CONTEXT('','3D')
);
#25069=(
GEOMETRIC_REPRESENTATION_CONTEXT(3)
GLOBAL_UNCERTAINTY_ASSIGNED_CONTEXT((#25035))
GLOBAL_UNIT_ASSIGNED_CONTEXT((#25075,#25077,#25078))
REPRESENTATION_CONTEXT('','3D')
);
#25070=(
GEOMETRIC_REPRESENTATION_CONTEXT(3)
GLOBAL_UNCERTAINTY_ASSIGNED_CONTEXT((#25036))
GLOBAL_UNIT_ASSIGNED_CONTEXT((#25075,#25077,#25078))
REPRESENTATION_CONTEXT('','3D')
);
#25071=(
GEOMETRIC_REPRESENTATION_CONTEXT(3)
GLOBAL_UNCERTAINTY_ASSIGNED_CONTEXT((#25037))
GLOBAL_UNIT_ASSIGNED_CONTEXT((#25075,#25077,#25078))
REPRESENTATION_CONTEXT('','3D')
);
#25072=(
GEOMETRIC_REPRESENTATION_CONTEXT(3)
GLOBAL_UNCERTAINTY_ASSIGNED_CONTEXT((#25038))
GLOBAL_UNIT_ASSIGNED_CONTEXT((#25075,#25077,#25078))
REPRESENTATION_CONTEXT('','3D')
);
#25073=(
GEOMETRIC_REPRESENTATION_CONTEXT(3)
GLOBAL_UNCERTAINTY_ASSIGNED_CONTEXT((#25039))
GLOBAL_UNIT_ASSIGNED_CONTEXT((#25075,#25077,#25078))
REPRESENTATION_CONTEXT('','3D')
);
#25074=(
GEOMETRIC_REPRESENTATION_CONTEXT(3)
GLOBAL_UNCERTAINTY_ASSIGNED_CONTEXT((#25040))
GLOBAL_UNIT_ASSIGNED_CONTEXT((#25075,#25077,#25078))
REPRESENTATION_CONTEXT('','3D')
);
#25075=(
LENGTH_UNIT()
NAMED_UNIT(*)
SI_UNIT(.CENTI.,.METRE.)
);
#25076=(
LENGTH_UNIT()
NAMED_UNIT(*)
SI_UNIT($,.METRE.)
);
#25077=(
NAMED_UNIT(*)
PLANE_ANGLE_UNIT()
SI_UNIT($,.RADIAN.)
);
#25078=(
NAMED_UNIT(*)
SI_UNIT($,.STERADIAN.)
SOLID_ANGLE_UNIT()
);
#25079=SHAPE_DEFINITION_REPRESENTATION(#25112,#25194);
#25080=SHAPE_DEFINITION_REPRESENTATION(#25113,#25195);
#25081=SHAPE_DEFINITION_REPRESENTATION(#25114,#25196);
#25082=SHAPE_DEFINITION_REPRESENTATION(#25115,#25197);
#25083=SHAPE_DEFINITION_REPRESENTATION(#25116,#25198);
#25084=SHAPE_DEFINITION_REPRESENTATION(#25117,#25199);
#25085=SHAPE_DEFINITION_REPRESENTATION(#25118,#25200);
#25086=SHAPE_DEFINITION_REPRESENTATION(#25119,#25201);
#25087=SHAPE_DEFINITION_REPRESENTATION(#25120,#25202);
#25088=SHAPE_DEFINITION_REPRESENTATION(#25121,#25203);
#25089=SHAPE_DEFINITION_REPRESENTATION(#25122,#25204);
#25090=SHAPE_DEFINITION_REPRESENTATION(#25123,#25205);
#25091=SHAPE_DEFINITION_REPRESENTATION(#25124,#25206);
#25092=SHAPE_DEFINITION_REPRESENTATION(#25125,#25207);
#25093=SHAPE_DEFINITION_REPRESENTATION(#25126,#25208);
#25094=SHAPE_DEFINITION_REPRESENTATION(#25132,#25209);
#25095=SHAPE_DEFINITION_REPRESENTATION(#25133,#25210);
#25096=SHAPE_DEFINITION_REPRESENTATION(#25134,#25211);
#25097=SHAPE_DEFINITION_REPRESENTATION(#25135,#25212);
#25098=SHAPE_DEFINITION_REPRESENTATION(#25136,#25213);
#25099=SHAPE_DEFINITION_REPRESENTATION(#25137,#25214);
#25100=SHAPE_DEFINITION_REPRESENTATION(#25138,#25215);
#25101=SHAPE_DEFINITION_REPRESENTATION(#25150,#25216);
#25102=SHAPE_DEFINITION_REPRESENTATION(#25151,#25217);
#25103=SHAPE_DEFINITION_REPRESENTATION(#25152,#25218);
#25104=SHAPE_DEFINITION_REPRESENTATION(#25153,#25219);
#25105=SHAPE_DEFINITION_REPRESENTATION(#25154,#25220);
#25106=SHAPE_DEFINITION_REPRESENTATION(#25155,#25221);
#25107=SHAPE_DEFINITION_REPRESENTATION(#25156,#25222);
#25108=SHAPE_DEFINITION_REPRESENTATION(#25157,#25223);
#25109=SHAPE_DEFINITION_REPRESENTATION(#25158,#25224);
#25110=SHAPE_DEFINITION_REPRESENTATION(#25159,#25225);
#25111=SHAPE_DEFINITION_REPRESENTATION(#25160,#25226);
#25112=PRODUCT_DEFINITION_SHAPE('',$,#25228);
#25113=PRODUCT_DEFINITION_SHAPE('',$,#25229);
#25114=PRODUCT_DEFINITION_SHAPE('',$,#25230);
#25115=PRODUCT_DEFINITION_SHAPE('',$,#25231);
#25116=PRODUCT_DEFINITION_SHAPE('',$,#25232);
#25117=PRODUCT_DEFINITION_SHAPE('',$,#25233);
#25118=PRODUCT_DEFINITION_SHAPE('',$,#25234);
#25119=PRODUCT_DEFINITION_SHAPE('',$,#25235);
#25120=PRODUCT_DEFINITION_SHAPE('',$,#25236);
#25121=PRODUCT_DEFINITION_SHAPE('',$,#25237);
#25122=PRODUCT_DEFINITION_SHAPE('',$,#25238);
#25123=PRODUCT_DEFINITION_SHAPE('',$,#25239);
#25124=PRODUCT_DEFINITION_SHAPE('',$,#25240);
#25125=PRODUCT_DEFINITION_SHAPE('',$,#25241);
#25126=PRODUCT_DEFINITION_SHAPE('',$,#25242);
#25127=PRODUCT_DEFINITION_SHAPE($,$,#162);
#25128=PRODUCT_DEFINITION_SHAPE($,$,#163);
#25129=PRODUCT_DEFINITION_SHAPE($,$,#164);
#25130=PRODUCT_DEFINITION_SHAPE($,$,#165);
#25131=PRODUCT_DEFINITION_SHAPE($,$,#166);
#25132=PRODUCT_DEFINITION_SHAPE('',$,#25243);
#25133=PRODUCT_DEFINITION_SHAPE('',$,#25244);
#25134=PRODUCT_DEFINITION_SHAPE('',$,#25245);
#25135=PRODUCT_DEFINITION_SHAPE('',$,#25246);
#25136=PRODUCT_DEFINITION_SHAPE('',$,#25247);
#25137=PRODUCT_DEFINITION_SHAPE('',$,#25248);
#25138=PRODUCT_DEFINITION_SHAPE('',$,#25249);
#25139=PRODUCT_DEFINITION_SHAPE($,$,#167);
#25140=PRODUCT_DEFINITION_SHAPE($,$,#168);
#25141=PRODUCT_DEFINITION_SHAPE($,$,#169);
#25142=PRODUCT_DEFINITION_SHAPE($,$,#170);
#25143=PRODUCT_DEFINITION_SHAPE($,$,#171);
#25144=PRODUCT_DEFINITION_SHAPE($,$,#172);
#25145=PRODUCT_DEFINITION_SHAPE($,$,#173);
#25146=PRODUCT_DEFINITION_SHAPE($,$,#174);
#25147=PRODUCT_DEFINITION_SHAPE($,$,#175);
#25148=PRODUCT_DEFINITION_SHAPE($,$,#176);
#25149=PRODUCT_DEFINITION_SHAPE($,$,#177);
#25150=PRODUCT_DEFINITION_SHAPE('',$,#25250);
#25151=PRODUCT_DEFINITION_SHAPE('',$,#25251);
#25152=PRODUCT_DEFINITION_SHAPE('',$,#25252);
#25153=PRODUCT_DEFINITION_SHAPE('',$,#25253);
#25154=PRODUCT_DEFINITION_SHAPE('',$,#25254);
#25155=PRODUCT_DEFINITION_SHAPE('',$,#25255);
#25156=PRODUCT_DEFINITION_SHAPE('',$,#25256);
#25157=PRODUCT_DEFINITION_SHAPE('',$,#25257);
#25158=PRODUCT_DEFINITION_SHAPE('',$,#25258);
#25159=PRODUCT_DEFINITION_SHAPE('',$,#25259);
#25160=PRODUCT_DEFINITION_SHAPE('',$,#25260);
#25161=PRODUCT_DEFINITION_SHAPE($,$,#178);
#25162=PRODUCT_DEFINITION_SHAPE($,$,#179);
#25163=PRODUCT_DEFINITION_SHAPE($,$,#180);
#25164=PRODUCT_DEFINITION_SHAPE($,$,#181);
#25165=PRODUCT_DEFINITION_SHAPE($,$,#182);
#25166=PRODUCT_DEFINITION_SHAPE($,$,#183);
#25167=PRODUCT_DEFINITION_SHAPE($,$,#184);
#25168=PRODUCT_DEFINITION_SHAPE($,$,#185);
#25169=PRODUCT_DEFINITION_SHAPE($,$,#186);
#25170=PRODUCT_DEFINITION_SHAPE($,$,#187);
#25171=PRODUCT_DEFINITION_SHAPE($,$,#188);
#25172=PRODUCT_DEFINITION_SHAPE($,$,#189);
#25173=PRODUCT_DEFINITION_SHAPE($,$,#190);
#25174=PRODUCT_DEFINITION_SHAPE($,$,#191);
#25175=PRODUCT_DEFINITION_SHAPE($,$,#192);
#25176=PRODUCT_DEFINITION_SHAPE($,$,#193);
#25177=PRODUCT_DEFINITION_SHAPE($,$,#194);
#25178=PRODUCT_DEFINITION_SHAPE($,$,#195);
#25179=PRODUCT_DEFINITION_SHAPE($,$,#196);
#25180=PRODUCT_DEFINITION_SHAPE($,$,#197);
#25181=PRODUCT_DEFINITION_SHAPE($,$,#198);
#25182=PRODUCT_DEFINITION_SHAPE($,$,#199);
#25183=PRODUCT_DEFINITION_SHAPE($,$,#200);
#25184=PRODUCT_DEFINITION_SHAPE($,$,#201);
#25185=PRODUCT_DEFINITION_SHAPE($,$,#202);
#25186=PRODUCT_DEFINITION_SHAPE($,$,#203);
#25187=PRODUCT_DEFINITION_SHAPE($,$,#204);
#25188=PRODUCT_DEFINITION_SHAPE($,$,#205);
#25189=PRODUCT_DEFINITION_SHAPE($,$,#206);
#25190=PRODUCT_DEFINITION_SHAPE($,$,#207);
#25191=PRODUCT_DEFINITION_SHAPE($,$,#208);
#25192=PRODUCT_DEFINITION_SHAPE($,$,#209);
#25193=PRODUCT_DEFINITION_SHAPE($,$,#210);
#25194=SHAPE_REPRESENTATION('',(#8401,#9201,#9202,#9203),#25041);
#25195=SHAPE_REPRESENTATION('',(#8402,#9171,#9172,#9173,#9174,#9175,#9176,
#9177,#9178,#9179,#9180,#9181,#9182,#9183,#9184,#9185,#9186,#9187,#9188,
#9189),#25042);
#25196=SHAPE_REPRESENTATION('',(#8403),#25043);
#25197=SHAPE_REPRESENTATION('',(#8431),#25044);
#25198=SHAPE_REPRESENTATION('',(#8450),#25045);
#25199=SHAPE_REPRESENTATION('',(#8473),#25046);
#25200=SHAPE_REPRESENTATION('',(#8504),#25047);
#25201=SHAPE_REPRESENTATION('',(#8527),#25048);
#25202=SHAPE_REPRESENTATION('',(#8548),#25049);
#25203=SHAPE_REPRESENTATION('',(#8572,#8701,#8702,#8703,#8704,#8705),#25050);
#25204=SHAPE_REPRESENTATION('',(#8573),#25051);
#25205=SHAPE_REPRESENTATION('',(#8593),#25052);
#25206=SHAPE_REPRESENTATION('',(#8613),#25053);
#25207=SHAPE_REPRESENTATION('',(#8630),#25054);
#25208=SHAPE_REPRESENTATION('',(#8684),#25055);
#25209=SHAPE_REPRESENTATION('',(#8706,#8880,#8881,#8882,#8883,#8884,#8885,
#8886,#8887,#8888,#8889,#8890),#25056);
#25210=SHAPE_REPRESENTATION('',(#8707),#25057);
#25211=SHAPE_REPRESENTATION('',(#8755),#25058);
#25212=SHAPE_REPRESENTATION('',(#8762),#25059);
#25213=SHAPE_REPRESENTATION('',(#8783),#25060);
#25214=SHAPE_REPRESENTATION('',(#8828),#25061);
#25215=SHAPE_REPRESENTATION('',(#8854),#25062);
#25216=SHAPE_REPRESENTATION('',(#8891,#9190,#9191,#9192,#9193,#9194,#9195,
#9196,#9197,#9198,#9199,#9200),#25063);
#25217=SHAPE_REPRESENTATION('',(#8892),#25064);
#25218=SHAPE_REPRESENTATION('',(#9043),#25065);
#25219=SHAPE_REPRESENTATION('',(#9052),#25066);
#25220=SHAPE_REPRESENTATION('',(#9066),#25067);
#25221=SHAPE_REPRESENTATION('',(#9090),#25068);
#25222=SHAPE_REPRESENTATION('',(#9099),#25069);
#25223=SHAPE_REPRESENTATION('',(#9108),#25070);
#25224=SHAPE_REPRESENTATION('',(#9119),#25071);
#25225=SHAPE_REPRESENTATION('',(#9136),#25072);
#25226=SHAPE_REPRESENTATION('',(#9145),#25073);
#25227=PRODUCT_DEFINITION_CONTEXT('part definition',#25328,'design');
#25228=PRODUCT_DEFINITION('PAT-024',
'PAT-024',#25261,#25227);
#25229=PRODUCT_DEFINITION('Fixed frame','Fixed frame',#25262,#25227);
#25230=PRODUCT_DEFINITION('Base','Base',#25263,#25227);
#25231=PRODUCT_DEFINITION('Dovetail guide','Dovetail guide',#25264,#25227);
#25232=PRODUCT_DEFINITION('Fixed jaw','Fixed jaw',#25265,#25227);
#25233=PRODUCT_DEFINITION('Bearing pedestal','Bearing pedestal',#25266,
#25227);
#25234=PRODUCT_DEFINITION('Bearing cap','Bearing cap',#25267,#25227);
#25235=PRODUCT_DEFINITION('Seventy-five millimetre jaw insert',
'Seventy-five millimetre jaw insert',#25268,#25227);
#25236=PRODUCT_DEFINITION('M6x20 trimmed screw','M6x20 trimmed screw',#25269,
#25227);
#25237=PRODUCT_DEFINITION('Sealed Ball Bearing - 20 x 47 x 14 mm',
'Sealed Ball Bearing - 20 x 47 x 14 mm',#25270,#25227);
#25238=PRODUCT_DEFINITION('Inner ring','Inner ring',#25271,#25227);
#25239=PRODUCT_DEFINITION('Outer ring','Outer ring',#25272,#25227);
#25240=PRODUCT_DEFINITION('Balls','Balls',#25273,#25227);
#25241=PRODUCT_DEFINITION('Cage','Cage',#25274,#25227);
#25242=PRODUCT_DEFINITION('Seals 2RS','Seals 2RS',#25275,#25227);
#25243=PRODUCT_DEFINITION('Moving jaw Assembly','Moving jaw Assembly',#25276,#25227);
#25244=PRODUCT_DEFINITION('Moving jaw','Moving jaw',#25277,#25227);
#25245=PRODUCT_DEFINITION('Gib','Gib',#25278,#25227);
#25246=PRODUCT_DEFINITION('Seventy-five millimetre jaw insert (1)',
'Seventy-five millimetre jaw insert (1)',#25279,#25227);
#25247=PRODUCT_DEFINITION('Flanged lead nut','Flanged lead nut',#25280,
#25227);
#25248=PRODUCT_DEFINITION('Cap Screw - M5x20','Cap Screw - M5x20',#25281,
#25227);
#25249=PRODUCT_DEFINITION('Cap Screw - M4x16','Cap Screw - M4x16',#25282,
#25227);
#25250=PRODUCT_DEFINITION('Screw and handwheel','Screw and handwheel',#25283,
#25227);
#25251=PRODUCT_DEFINITION('Tr12x3 lead screw','Tr12x3 lead screw',#25284,
#25227);
#25252=PRODUCT_DEFINITION('Inner race spacer','Inner race spacer',#25285,
#25227);
#25253=PRODUCT_DEFINITION('Shaft retaining collar',
'Shaft retaining collar',#25286,#25227);
#25254=PRODUCT_DEFINITION('Handwheel','Handwheel',#25287,#25227);
#25255=PRODUCT_DEFINITION('Handle pivot sleeve','Handle pivot sleeve',#25288,
#25227);
#25256=PRODUCT_DEFINITION('Revolving handle','Revolving handle',#25289,
#25227);
#25257=PRODUCT_DEFINITION('Key 6x6x20','Key 6x6x20',#25290,#25227);
#25258=PRODUCT_DEFINITION('Socket Set Screw - M5x8',
'Socket Set Screw - M5x8',#25291,#25227);
#25259=PRODUCT_DEFINITION('Flat Washer - M6','Flat Washer - M6',#25292,
#25227);
#25260=PRODUCT_DEFINITION('Cap Screw - M6x25','Cap Screw - M6x25',#25293,
#25227);
#25261=PRODUCT_DEFINITION_FORMATION('',$,#25330);
#25262=PRODUCT_DEFINITION_FORMATION('',$,#25331);
#25263=PRODUCT_DEFINITION_FORMATION('',$,#25332);
#25264=PRODUCT_DEFINITION_FORMATION('',$,#25333);
#25265=PRODUCT_DEFINITION_FORMATION('',$,#25334);
#25266=PRODUCT_DEFINITION_FORMATION('',$,#25335);
#25267=PRODUCT_DEFINITION_FORMATION('',$,#25336);
#25268=PRODUCT_DEFINITION_FORMATION('',$,#25337);
#25269=PRODUCT_DEFINITION_FORMATION('',$,#25338);
#25270=PRODUCT_DEFINITION_FORMATION('',$,#25339);
#25271=PRODUCT_DEFINITION_FORMATION('',$,#25340);
#25272=PRODUCT_DEFINITION_FORMATION('',$,#25341);
#25273=PRODUCT_DEFINITION_FORMATION('',$,#25342);
#25274=PRODUCT_DEFINITION_FORMATION('',$,#25343);
#25275=PRODUCT_DEFINITION_FORMATION('',$,#25344);
#25276=PRODUCT_DEFINITION_FORMATION('',$,#25345);
#25277=PRODUCT_DEFINITION_FORMATION('',$,#25346);
#25278=PRODUCT_DEFINITION_FORMATION('',$,#25347);
#25279=PRODUCT_DEFINITION_FORMATION('',$,#25348);
#25280=PRODUCT_DEFINITION_FORMATION('',$,#25349);
#25281=PRODUCT_DEFINITION_FORMATION('',$,#25350);
#25282=PRODUCT_DEFINITION_FORMATION('',$,#25351);
#25283=PRODUCT_DEFINITION_FORMATION('',$,#25352);
#25284=PRODUCT_DEFINITION_FORMATION('',$,#25353);
#25285=PRODUCT_DEFINITION_FORMATION('',$,#25354);
#25286=PRODUCT_DEFINITION_FORMATION('',$,#25355);
#25287=PRODUCT_DEFINITION_FORMATION('',$,#25356);
#25288=PRODUCT_DEFINITION_FORMATION('',$,#25357);
#25289=PRODUCT_DEFINITION_FORMATION('',$,#25358);
#25290=PRODUCT_DEFINITION_FORMATION('',$,#25359);
#25291=PRODUCT_DEFINITION_FORMATION('',$,#25360);
#25292=PRODUCT_DEFINITION_FORMATION('',$,#25361);
#25293=PRODUCT_DEFINITION_FORMATION('',$,#25362);
#25294=PRODUCT_RELATED_PRODUCT_CATEGORY('PAT-024',
'PAT-024',(#25330));
#25295=PRODUCT_RELATED_PRODUCT_CATEGORY('Fixed frame','Fixed frame',(#25331));
#25296=PRODUCT_RELATED_PRODUCT_CATEGORY('Base','Base',(#25332));
#25297=PRODUCT_RELATED_PRODUCT_CATEGORY('Dovetail guide',
'Dovetail guide',(#25333));
#25298=PRODUCT_RELATED_PRODUCT_CATEGORY('Fixed jaw','Fixed jaw',(#25334));
#25299=PRODUCT_RELATED_PRODUCT_CATEGORY('Bearing pedestal',
'Bearing pedestal',(#25335));
#25300=PRODUCT_RELATED_PRODUCT_CATEGORY('Bearing cap','Bearing cap',(#25336));
#25301=PRODUCT_RELATED_PRODUCT_CATEGORY(
'Seventy-five millimetre jaw insert',
'Seventy-five millimetre jaw insert',(#25337));
#25302=PRODUCT_RELATED_PRODUCT_CATEGORY('M6x20 trimmed screw',
'M6x20 trimmed screw',(#25338));
#25303=PRODUCT_RELATED_PRODUCT_CATEGORY(
'Sealed Ball Bearing - 20 x 47 x 14 mm',
'Sealed Ball Bearing - 20 x 47 x 14 mm',(#25339));
#25304=PRODUCT_RELATED_PRODUCT_CATEGORY('Inner ring','Inner ring',(#25340));
#25305=PRODUCT_RELATED_PRODUCT_CATEGORY('Outer ring','Outer ring',(#25341));
#25306=PRODUCT_RELATED_PRODUCT_CATEGORY('Balls','Balls',(#25342));
#25307=PRODUCT_RELATED_PRODUCT_CATEGORY('Cage','Cage',(#25343));
#25308=PRODUCT_RELATED_PRODUCT_CATEGORY('Seals 2RS','Seals 2RS',(#25344));
#25309=PRODUCT_RELATED_PRODUCT_CATEGORY('Moving jaw Assembly',
'Moving jaw Assembly',(#25345));
#25310=PRODUCT_RELATED_PRODUCT_CATEGORY('Moving jaw','Moving jaw',(#25346));
#25311=PRODUCT_RELATED_PRODUCT_CATEGORY('Gib','Gib',(#25347));
#25312=PRODUCT_RELATED_PRODUCT_CATEGORY(
'Seventy-five millimetre jaw insert (1)',
'Seventy-five millimetre jaw insert (1)',(#25348));
#25313=PRODUCT_RELATED_PRODUCT_CATEGORY('Flanged lead nut',
'Flanged lead nut',(#25349));
#25314=PRODUCT_RELATED_PRODUCT_CATEGORY('Cap Screw - M5x20',
'Cap Screw - M5x20',(#25350));
#25315=PRODUCT_RELATED_PRODUCT_CATEGORY('Cap Screw - M4x16',
'Cap Screw - M4x16',(#25351));
#25316=PRODUCT_RELATED_PRODUCT_CATEGORY('Screw and handwheel',
'Screw and handwheel',(#25352));
#25317=PRODUCT_RELATED_PRODUCT_CATEGORY('Tr12x3 lead screw',
'Tr12x3 lead screw',(#25353));
#25318=PRODUCT_RELATED_PRODUCT_CATEGORY('Inner race spacer',
'Inner race spacer',(#25354));
#25319=PRODUCT_RELATED_PRODUCT_CATEGORY('Shaft retaining collar',
'Shaft retaining collar',(#25355));
#25320=PRODUCT_RELATED_PRODUCT_CATEGORY('Handwheel','Handwheel',(#25356));
#25321=PRODUCT_RELATED_PRODUCT_CATEGORY('Handle pivot sleeve',
'Handle pivot sleeve',(#25357));
#25322=PRODUCT_RELATED_PRODUCT_CATEGORY('Revolving handle',
'Revolving handle',(#25358));
#25323=PRODUCT_RELATED_PRODUCT_CATEGORY('Key 6x6x20','Key 6x6x20',(#25359));
#25324=PRODUCT_RELATED_PRODUCT_CATEGORY('Socket Set Screw - M5x8',
'Socket Set Screw - M5x8',(#25360));
#25325=PRODUCT_RELATED_PRODUCT_CATEGORY('Flat Washer - M6',
'Flat Washer - M6',(#25361));
#25326=PRODUCT_RELATED_PRODUCT_CATEGORY('Cap Screw - M6x25',
'Cap Screw - M6x25',(#25362));
#25327=APPLICATION_PROTOCOL_DEFINITION('international standard',
'automotive_design',2009,#25328);
#25328=APPLICATION_CONTEXT(
'Core Data for Automotive Mechanical Design Process');
#25329=PRODUCT_CONTEXT('part definition',#25328,'mechanical');
#25330=PRODUCT('PAT-024','PAT-024',
'PAT-024',(#25329));
#25331=PRODUCT('Fixed frame','Fixed frame','Fixed frame',(#25329));
#25332=PRODUCT('Base','Base','Base',(#25329));
#25333=PRODUCT('Dovetail guide','Dovetail guide','Dovetail guide',(#25329));
#25334=PRODUCT('Fixed jaw','Fixed jaw','Fixed jaw',(#25329));
#25335=PRODUCT('Bearing pedestal','Bearing pedestal','Bearing pedestal',
(#25329));
#25336=PRODUCT('Bearing cap','Bearing cap','Bearing cap',(#25329));
#25337=PRODUCT('Seventy-five millimetre jaw insert',
'Seventy-five millimetre jaw insert',
'Seventy-five millimetre jaw insert',(#25329));
#25338=PRODUCT('M6x20 trimmed screw','M6x20 trimmed screw',
'M6x20 trimmed screw',(#25329));
#25339=PRODUCT('Sealed Ball Bearing - 20 x 47 x 14 mm',
'Sealed Ball Bearing - 20 x 47 x 14 mm',
'Sealed Ball Bearing - 20 x 47 x 14 mm',(#25329));
#25340=PRODUCT('Inner ring','Inner ring','Inner ring',(#25329));
#25341=PRODUCT('Outer ring','Outer ring','Outer ring',(#25329));
#25342=PRODUCT('Balls','Balls','Balls',(#25329));
#25343=PRODUCT('Cage','Cage','Cage',(#25329));
#25344=PRODUCT('Seals 2RS','Seals 2RS','Seals 2RS',(#25329));
#25345=PRODUCT('Moving jaw Assembly','Moving jaw Assembly','Moving jaw Assembly',(#25329));
#25346=PRODUCT('Moving jaw','Moving jaw','Moving jaw',(#25329));
#25347=PRODUCT('Gib','Gib','Gib',(#25329));
#25348=PRODUCT('Seventy-five millimetre jaw insert (1)',
'Seventy-five millimetre jaw insert (1)',
'Seventy-five millimetre jaw insert (1)',(#25329));
#25349=PRODUCT('Flanged lead nut','Flanged lead nut','Flanged lead nut',
(#25329));
#25350=PRODUCT('Cap Screw - M5x20','Cap Screw - M5x20',
'Cap Screw - M5x20',(#25329));
#25351=PRODUCT('Cap Screw - M4x16','Cap Screw - M4x16',
'Cap Screw - M4x16',(#25329));
#25352=PRODUCT('Screw and handwheel','Screw and handwheel',
'Screw and handwheel',(#25329));
#25353=PRODUCT('Tr12x3 lead screw','Tr12x3 lead screw',
'Tr12x3 lead screw',(#25329));
#25354=PRODUCT('Inner race spacer','Inner race spacer',
'Inner race spacer',(#25329));
#25355=PRODUCT('Shaft retaining collar','Shaft retaining collar',
'Shaft retaining collar',(#25329));
#25356=PRODUCT('Handwheel','Handwheel','Handwheel',(#25329));
#25357=PRODUCT('Handle pivot sleeve','Handle pivot sleeve',
'Handle pivot sleeve',(#25329));
#25358=PRODUCT('Revolving handle','Revolving handle','Revolving handle',
(#25329));
#25359=PRODUCT('Key 6x6x20','Key 6x6x20','Key 6x6x20',(#25329));
#25360=PRODUCT('Socket Set Screw - M5x8','Socket Set Screw - M5x8',
'Socket Set Screw - M5x8',(#25329));
#25361=PRODUCT('Flat Washer - M6','Flat Washer - M6','Flat Washer - M6',
(#25329));
#25362=PRODUCT('Cap Screw - M6x25','Cap Screw - M6x25',
'Cap Screw - M6x25',(#25329));
#25363=PRESENTATION_STYLE_ASSIGNMENT((#25370));
#25364=PRESENTATION_STYLE_ASSIGNMENT((#25371));
#25365=PRESENTATION_STYLE_ASSIGNMENT((#25372));
#25366=PRESENTATION_STYLE_ASSIGNMENT((#25373));
#25367=PRESENTATION_STYLE_ASSIGNMENT((#25374));
#25368=PRESENTATION_STYLE_ASSIGNMENT((#25375));
#25369=PRESENTATION_STYLE_ASSIGNMENT((#25376));
#25370=SURFACE_STYLE_USAGE(.BOTH.,#25377);
#25371=SURFACE_STYLE_USAGE(.BOTH.,#25378);
#25372=SURFACE_STYLE_USAGE(.BOTH.,#25379);
#25373=SURFACE_STYLE_USAGE(.BOTH.,#25380);
#25374=SURFACE_STYLE_USAGE(.BOTH.,#25381);
#25375=SURFACE_STYLE_USAGE(.BOTH.,#25382);
#25376=SURFACE_STYLE_USAGE(.BOTH.,#25383);
#25377=SURFACE_SIDE_STYLE('',(#25384));
#25378=SURFACE_SIDE_STYLE('',(#25385));
#25379=SURFACE_SIDE_STYLE('',(#25386));
#25380=SURFACE_SIDE_STYLE('',(#25387));
#25381=SURFACE_SIDE_STYLE('',(#25388));
#25382=SURFACE_SIDE_STYLE('',(#25389));
#25383=SURFACE_SIDE_STYLE('',(#25390));
#25384=SURFACE_STYLE_FILL_AREA(#25391);
#25385=SURFACE_STYLE_FILL_AREA(#25392);
#25386=SURFACE_STYLE_FILL_AREA(#25393);
#25387=SURFACE_STYLE_FILL_AREA(#25394);
#25388=SURFACE_STYLE_FILL_AREA(#25395);
#25389=SURFACE_STYLE_FILL_AREA(#25396);
#25390=SURFACE_STYLE_FILL_AREA(#25397);
#25391=FILL_AREA_STYLE('Steel - Satin',(#25398));
#25392=FILL_AREA_STYLE('CAD Library Painted - Deep blue',(#25399));
#25393=FILL_AREA_STYLE('CAD Library Painted - Engineering blue',(#25400));
#25394=FILL_AREA_STYLE('CAD Library Painted - Steel gray',(#25401));
#25395=FILL_AREA_STYLE('CAD Library Painted - Graphite',(#25402));
#25396=FILL_AREA_STYLE('CAD Library Painted - Off white',(#25403));
#25397=FILL_AREA_STYLE('CAD Library Painted - Light blue',(#25404));
#25398=FILL_AREA_STYLE_COLOUR('Steel - Satin',#25405);
#25399=FILL_AREA_STYLE_COLOUR('CAD Library Painted - Deep blue',#25406);
#25400=FILL_AREA_STYLE_COLOUR('CAD Library Painted - Engineering blue',
#25407);
#25401=FILL_AREA_STYLE_COLOUR('CAD Library Painted - Steel gray',#25408);
#25402=FILL_AREA_STYLE_COLOUR('CAD Library Painted - Graphite',#25409);
#25403=FILL_AREA_STYLE_COLOUR('CAD Library Painted - Off white',#25410);
#25404=FILL_AREA_STYLE_COLOUR('CAD Library Painted - Light blue',#25411);
#25405=COLOUR_RGB('Steel - Satin',0.627450980392157,0.627450980392157,0.627450980392157);
#25406=COLOUR_RGB('CAD Library Painted - Deep blue',0.0784313725490196,
0.203921568627451,0.349019607843137);
#25407=COLOUR_RGB('CAD Library Painted - Engineering blue',0.12156862745098,
0.356862745098039,0.6);
#25408=COLOUR_RGB('CAD Library Painted - Steel gray',0.592156862745098,
0.631372549019608,0.67843137254902);
#25409=COLOUR_RGB('CAD Library Painted - Graphite',0.0980392156862745,0.109803921568627,
0.125490196078431);
#25410=COLOUR_RGB('CAD Library Painted - Off white',0.909803921568627,0.901960784313726,
0.858823529411765);
#25411=COLOUR_RGB('CAD Library Painted - Light blue',0.286274509803922,
0.552941176470588,0.780392156862745);
#25412=COLOUR_RGB('Dark Blue',0.08,0.2,0.34);
#25413=FILL_AREA_STYLE_COLOUR('',#25412);
#25414=FILL_AREA_STYLE('',(#25413));
#25415=SURFACE_STYLE_FILL_AREA(#25414);
#25416=SURFACE_SIDE_STYLE('',(#25415));
#25417=SURFACE_STYLE_USAGE(.BOTH.,#25416);
#25418=PRESENTATION_STYLE_ASSIGNMENT((#25417));
#25419=COLOUR_RGB('Light Blue',0.38,0.62,0.78);
#25420=FILL_AREA_STYLE_COLOUR('',#25419);
#25421=FILL_AREA_STYLE('',(#25420));
#25422=SURFACE_STYLE_FILL_AREA(#25421);
#25423=SURFACE_SIDE_STYLE('',(#25422));
#25424=SURFACE_STYLE_USAGE(.BOTH.,#25423);
#25425=PRESENTATION_STYLE_ASSIGNMENT((#25424));
#25426=COLOUR_RGB('Sky Blue',0.24,0.69,0.87);
#25427=FILL_AREA_STYLE_COLOUR('',#25426);
#25428=FILL_AREA_STYLE('',(#25427));
#25429=SURFACE_STYLE_FILL_AREA(#25428);
#25430=SURFACE_SIDE_STYLE('',(#25429));
#25431=SURFACE_STYLE_USAGE(.BOTH.,#25430);
#25432=PRESENTATION_STYLE_ASSIGNMENT((#25431));
#25433=COLOUR_RGB('Grey',0.48,0.52,0.57);
#25434=FILL_AREA_STYLE_COLOUR('',#25433);
#25435=FILL_AREA_STYLE('',(#25434));
#25436=SURFACE_STYLE_FILL_AREA(#25435);
#25437=SURFACE_SIDE_STYLE('',(#25436));
#25438=SURFACE_STYLE_USAGE(.BOTH.,#25437);
#25439=PRESENTATION_STYLE_ASSIGNMENT((#25438));
#25440=COLOUR_RGB('Black',0.12,0.14,0.17);
#25441=FILL_AREA_STYLE_COLOUR('',#25440);
#25442=FILL_AREA_STYLE('',(#25441));
#25443=SURFACE_STYLE_FILL_AREA(#25442);
#25444=SURFACE_SIDE_STYLE('',(#25443));
#25445=SURFACE_STYLE_USAGE(.BOTH.,#25444);
#25446=PRESENTATION_STYLE_ASSIGNMENT((#25445));
#25447=COLOUR_RGB('Off White',0.89,0.88,0.83);
#25448=FILL_AREA_STYLE_COLOUR('',#25447);
#25449=FILL_AREA_STYLE('',(#25448));
#25450=SURFACE_STYLE_FILL_AREA(#25449);
#25451=SURFACE_SIDE_STYLE('',(#25450));
#25452=SURFACE_STYLE_USAGE(.BOTH.,#25451);
#25453=PRESENTATION_STYLE_ASSIGNMENT((#25452));
ENDSEC;
END-ISO-10303-21;
